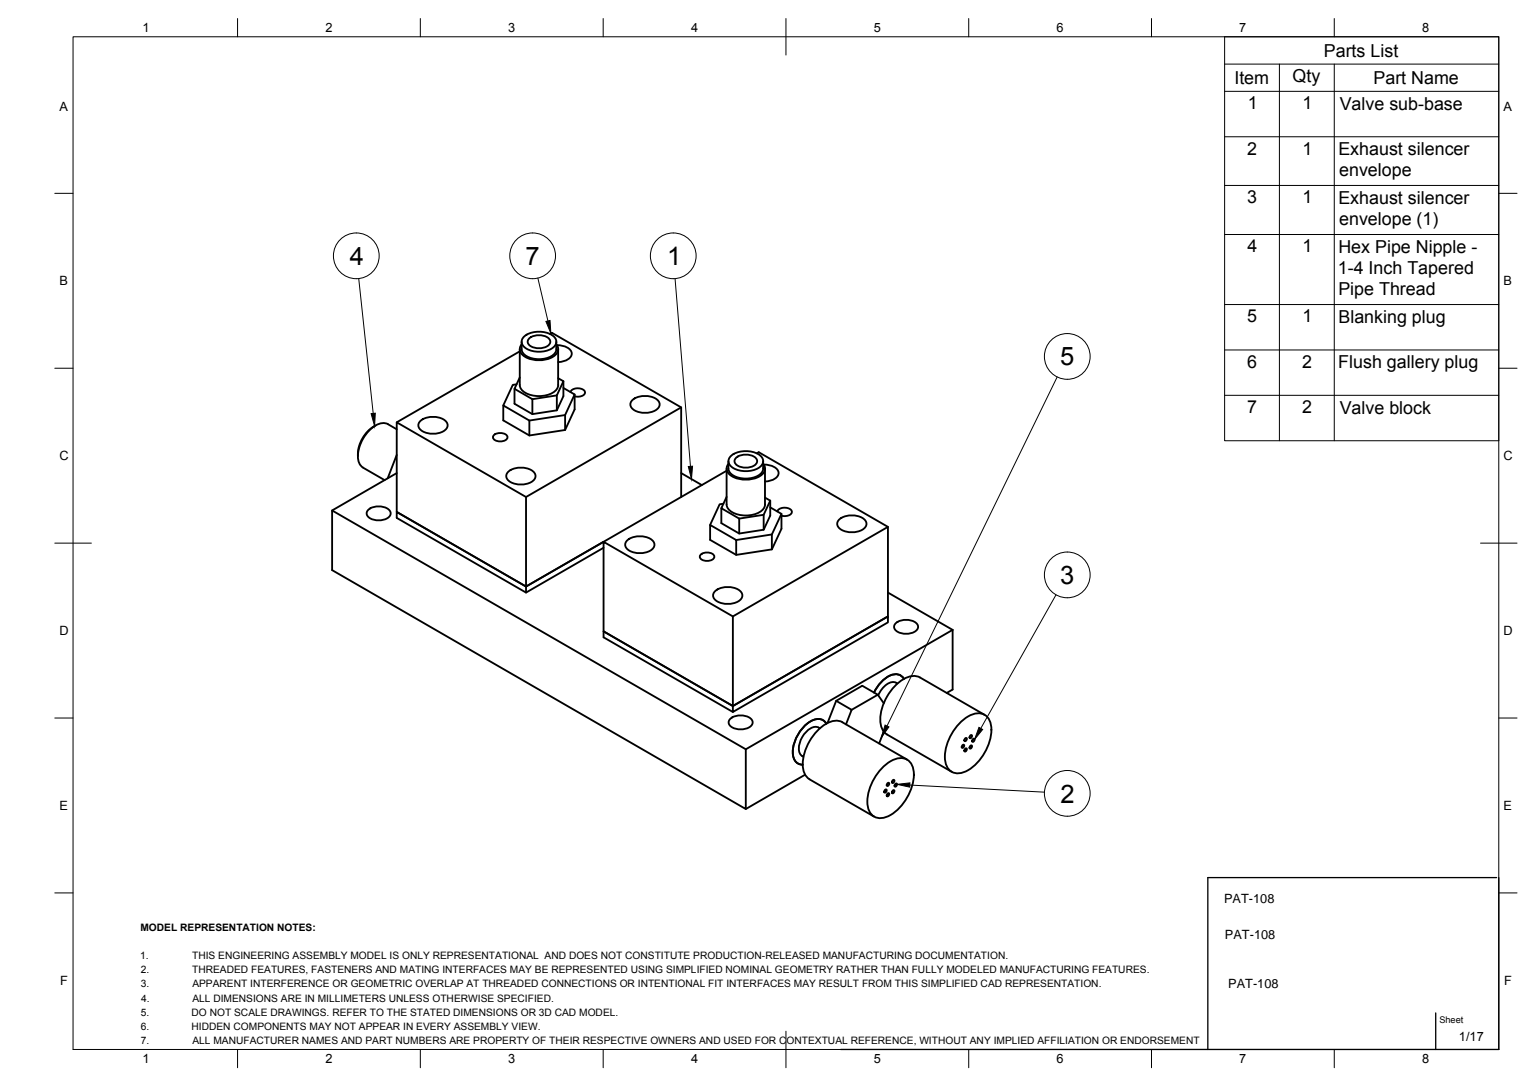
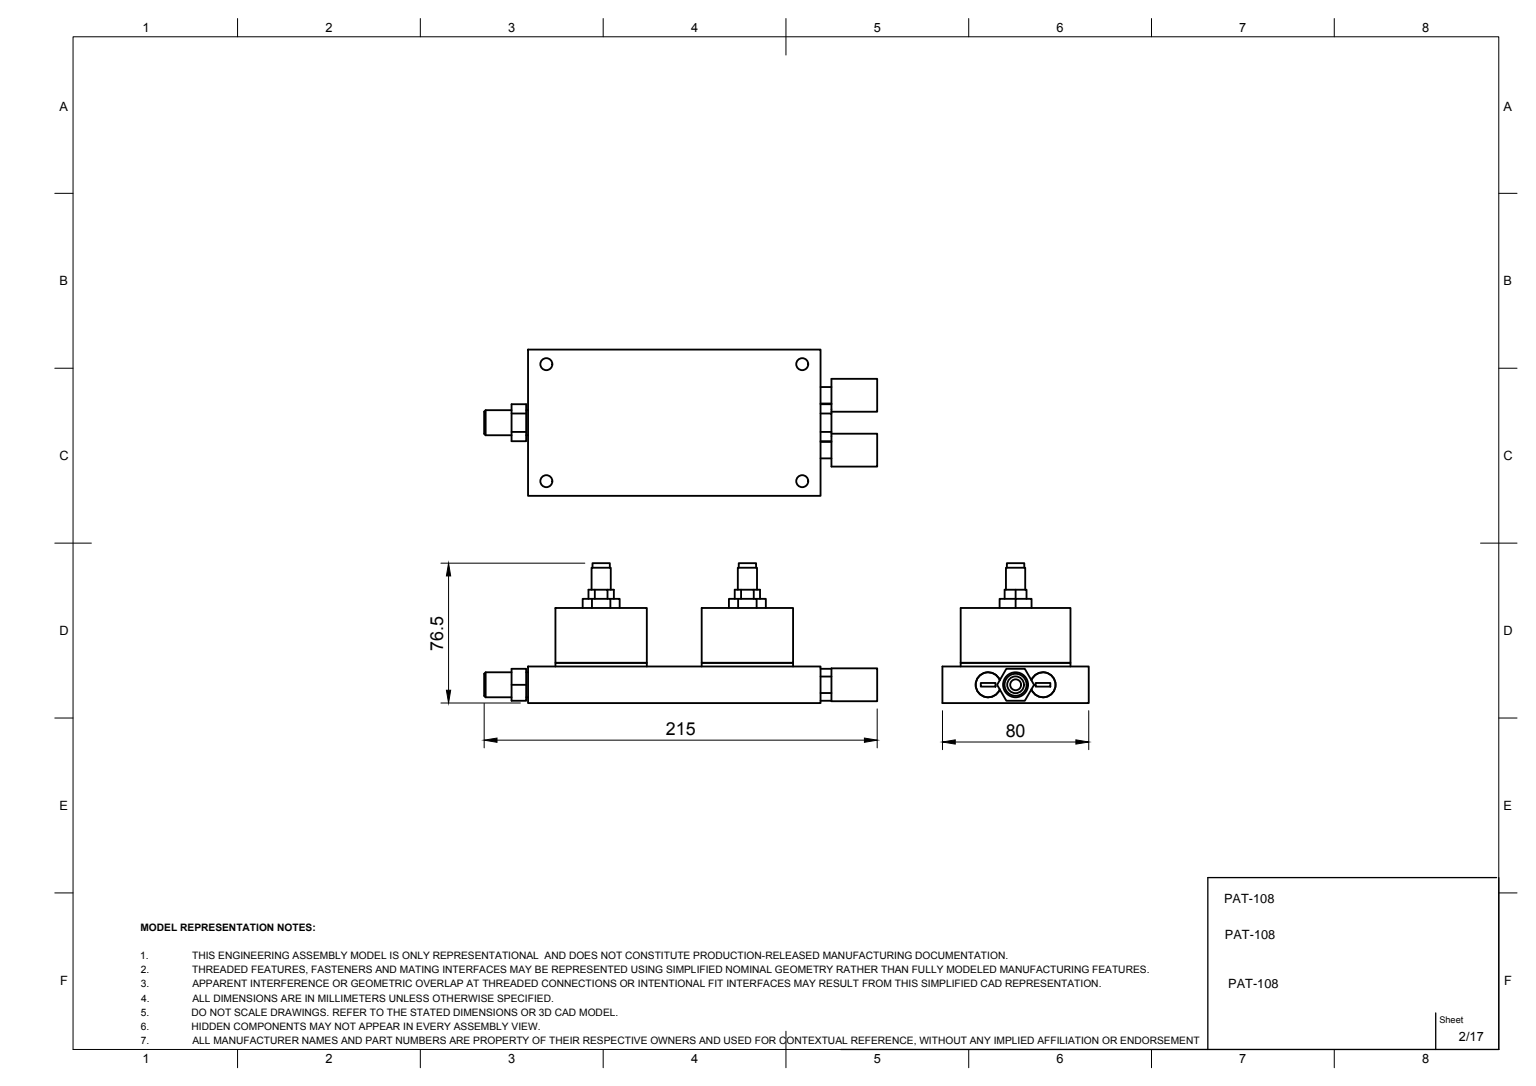
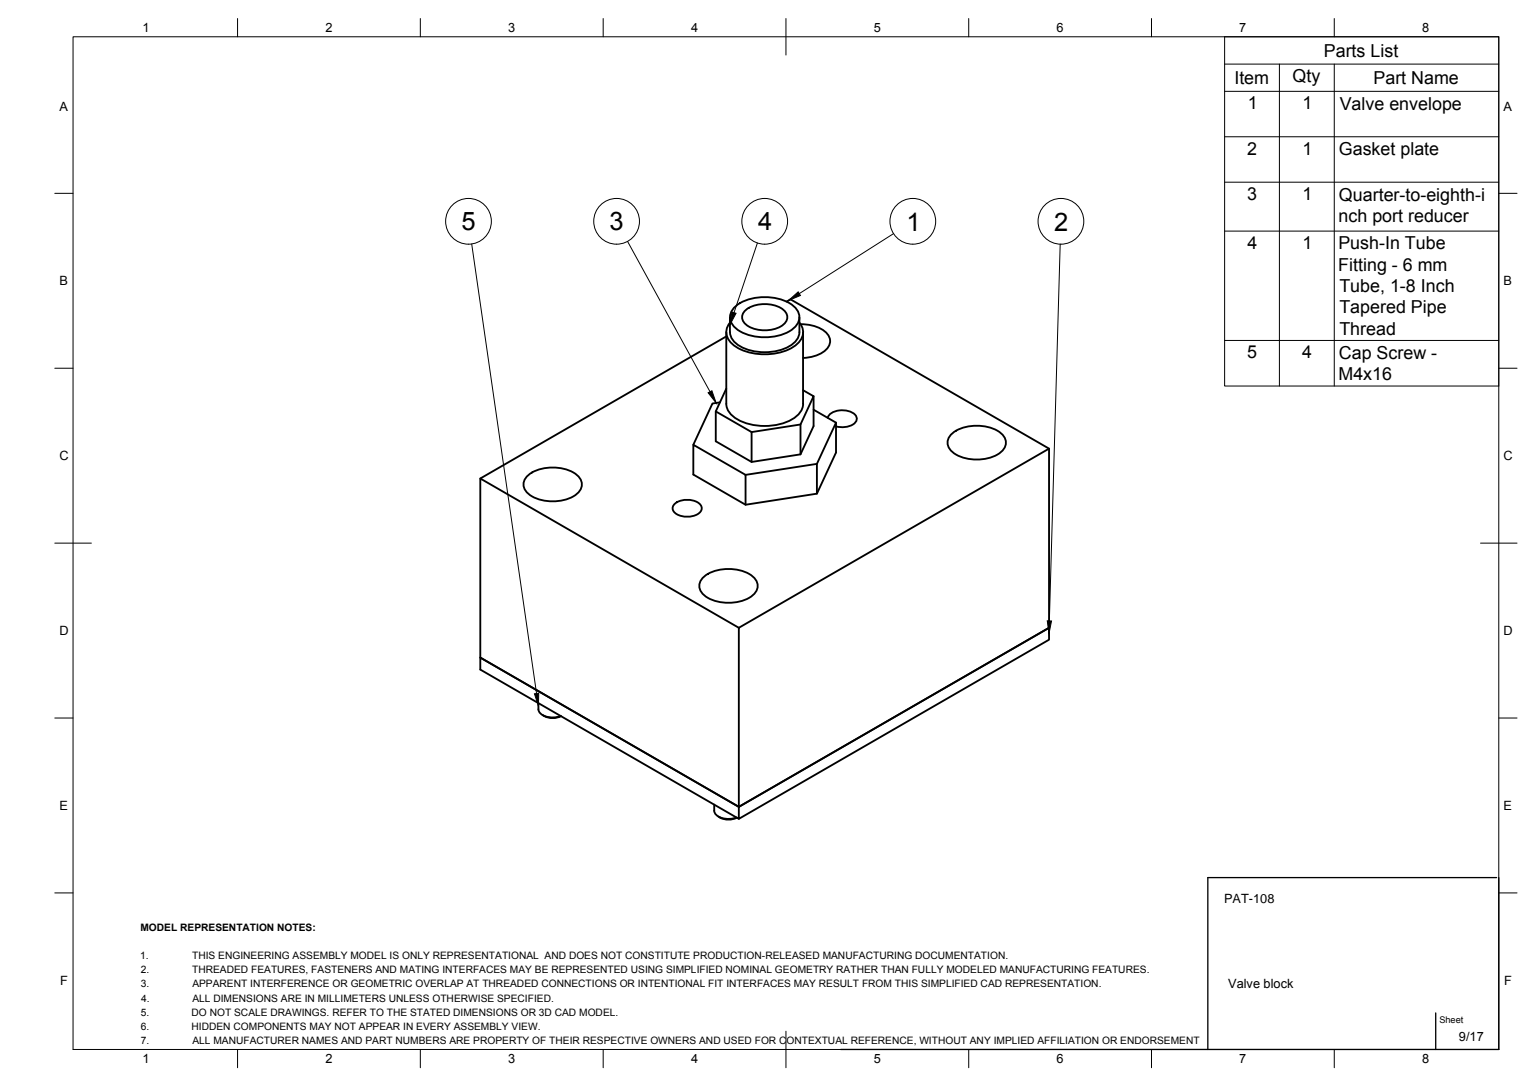
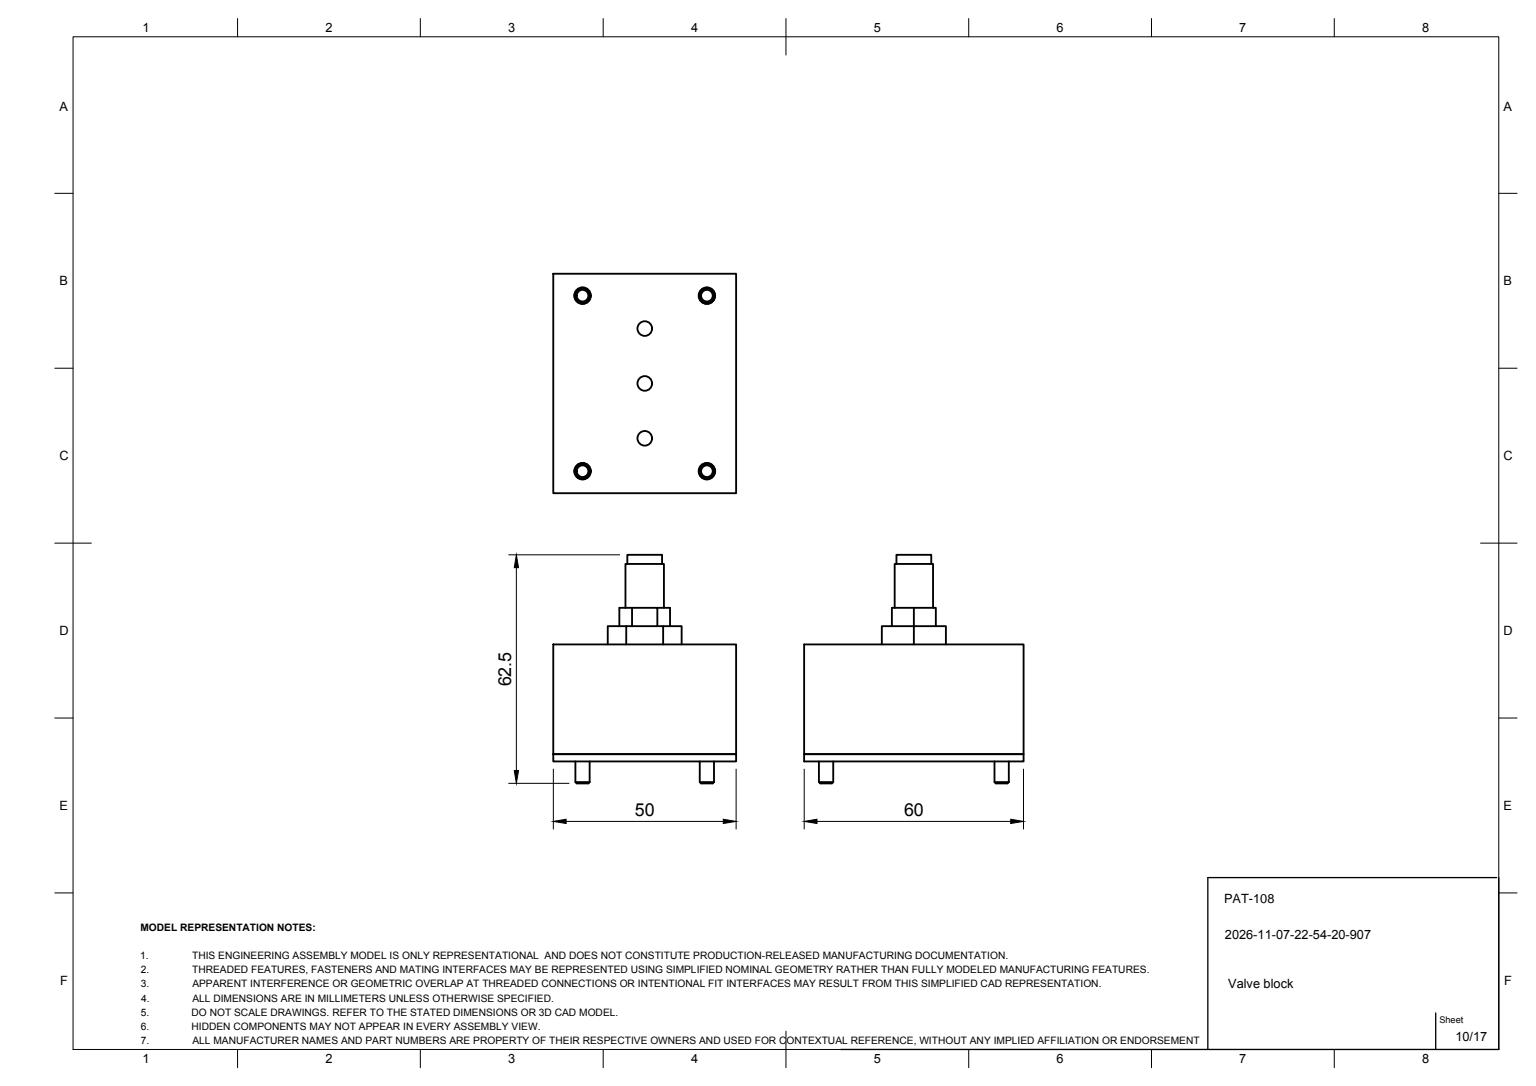
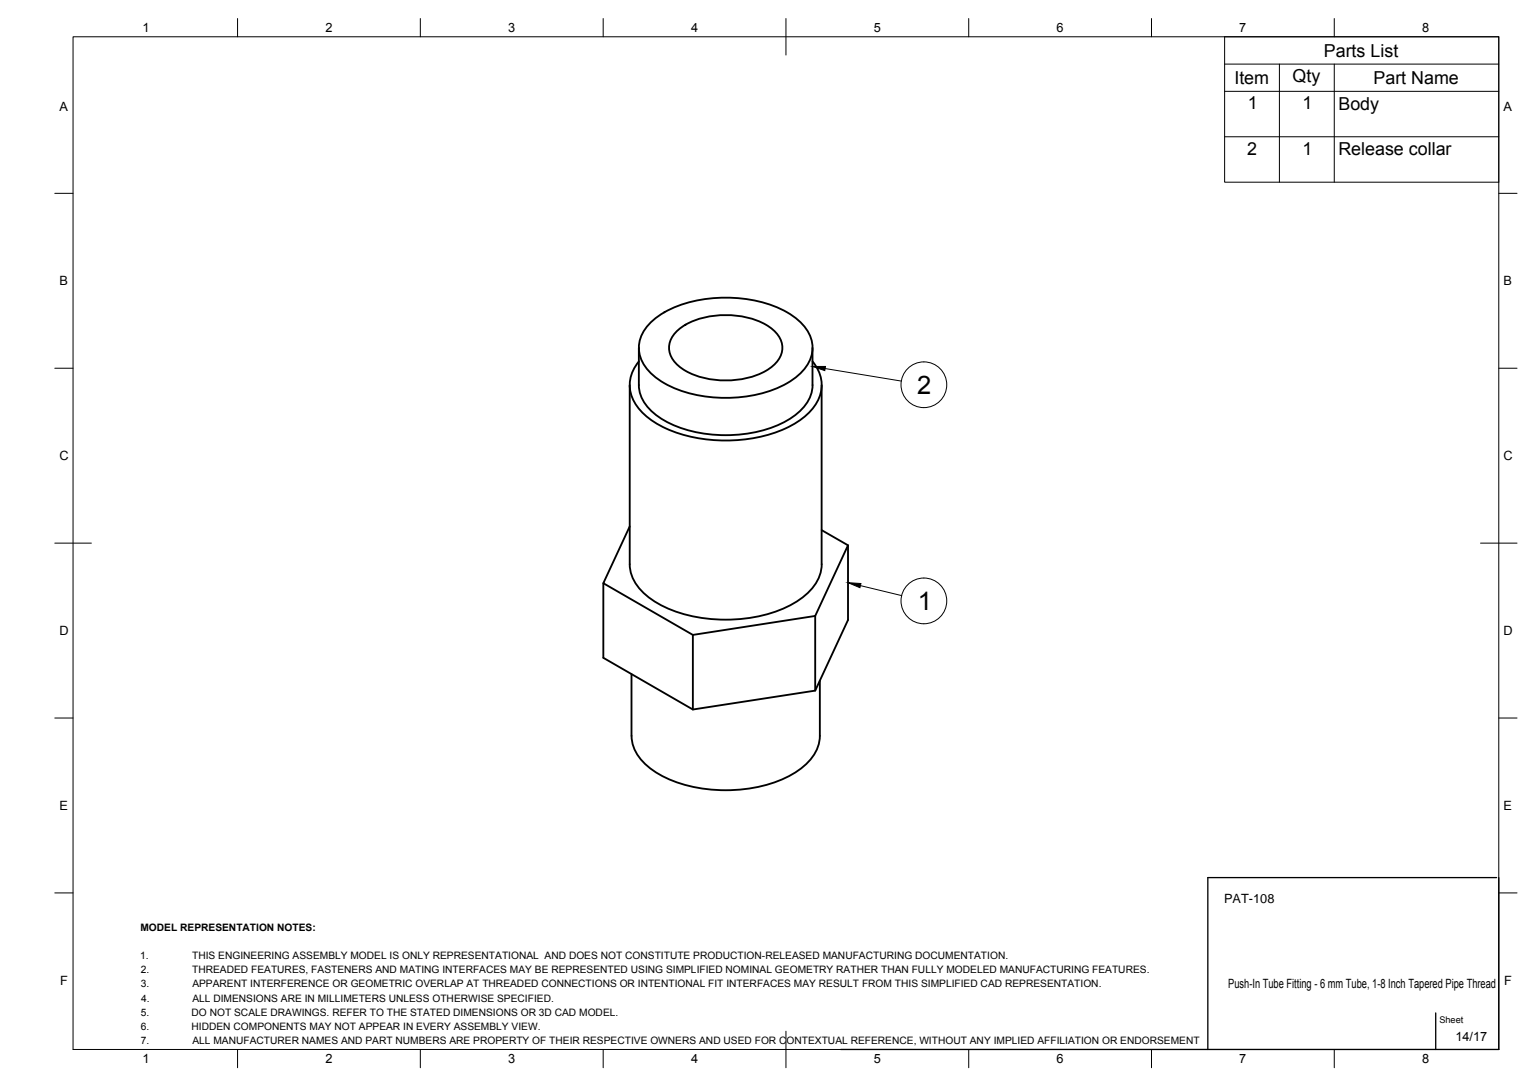
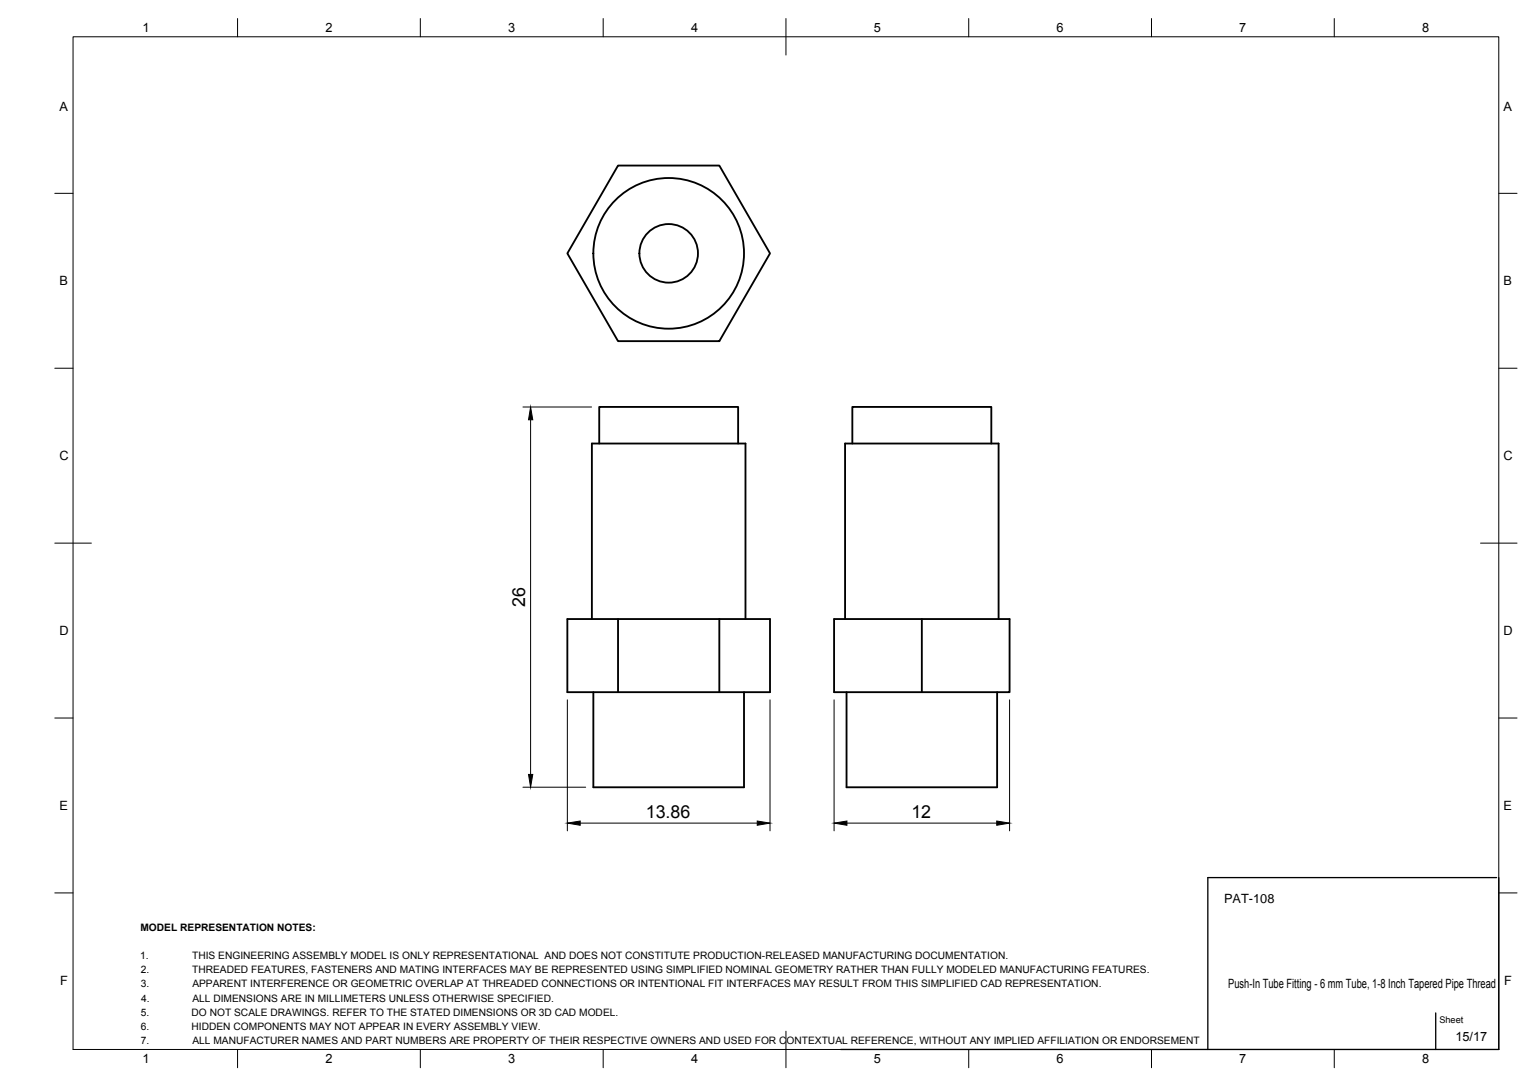
ISO-10303-21;
HEADER;
/* Generated by software containing ST-Developer
 * from STEP Tools, Inc. (www.steptools.com) 
 */

FILE_DESCRIPTION(
/* description */ ('Sub-base valve envelopes and connections'),
/* implementation_level */ '2;1');

FILE_NAME(
/* name */ 'PAT-108',
/* time_stamp */ '2026-10-29T15:55:44-07:00',
/* author */ (''),
/* organization */ (''),
/* preprocessor_version */ 'ST-DEVELOPER v20.2',
/* originating_system */ 'Autodesk Translation Framework v15.17.0.0',
/* authorisation */ '');

FILE_SCHEMA (('AUTOMOTIVE_DESIGN { 1 0 10303 214 3 1 1 }'));
ENDSEC;

DATA;
#10=MECHANICAL_DESIGN_GEOMETRIC_PRESENTATION_REPRESENTATION('',(#119,#120,
#121,#122,#123,#124,#125,#126,#127,#128,#129,#130),#6113);
#11=ORIENTED_CLOSED_SHELL('',*,#3370,.F.);
#12=BREP_WITH_VOIDS('Body1',#3369,(#11));
#13=ITEM_DEFINED_TRANSFORMATION($,$,#3819,#3860);
#14=ITEM_DEFINED_TRANSFORMATION($,$,#3847,#3861);
#15=ITEM_DEFINED_TRANSFORMATION($,$,#3722,#3888);
#16=ITEM_DEFINED_TRANSFORMATION($,$,#3770,#3889);
#17=ITEM_DEFINED_TRANSFORMATION($,$,#3798,#3890);
#18=ITEM_DEFINED_TRANSFORMATION($,$,#3818,#3891);
#19=ITEM_DEFINED_TRANSFORMATION($,$,#3862,#3892);
#20=ITEM_DEFINED_TRANSFORMATION($,$,#3862,#3893);
#21=ITEM_DEFINED_TRANSFORMATION($,$,#3862,#3894);
#22=ITEM_DEFINED_TRANSFORMATION($,$,#3862,#3895);
#23=ITEM_DEFINED_TRANSFORMATION($,$,#3505,#3896);
#24=ITEM_DEFINED_TRANSFORMATION($,$,#3601,#3897);
#25=ITEM_DEFINED_TRANSFORMATION($,$,#3637,#3898);
#26=ITEM_DEFINED_TRANSFORMATION($,$,#3673,#3899);
#27=ITEM_DEFINED_TRANSFORMATION($,$,#3697,#3900);
#28=ITEM_DEFINED_TRANSFORMATION($,$,#3710,#3901);
#29=ITEM_DEFINED_TRANSFORMATION($,$,#3710,#3902);
#30=ITEM_DEFINED_TRANSFORMATION($,$,#3721,#3903);
#31=ITEM_DEFINED_TRANSFORMATION($,$,#3721,#3904);
#32=(
REPRESENTATION_RELATIONSHIP($,$,#6179,#6178)
REPRESENTATION_RELATIONSHIP_WITH_TRANSFORMATION(#13)
SHAPE_REPRESENTATION_RELATIONSHIP()
);
#33=(
REPRESENTATION_RELATIONSHIP($,$,#6180,#6178)
REPRESENTATION_RELATIONSHIP_WITH_TRANSFORMATION(#14)
SHAPE_REPRESENTATION_RELATIONSHIP()
);
#34=(
REPRESENTATION_RELATIONSHIP($,$,#6175,#6174)
REPRESENTATION_RELATIONSHIP_WITH_TRANSFORMATION(#15)
SHAPE_REPRESENTATION_RELATIONSHIP()
);
#35=(
REPRESENTATION_RELATIONSHIP($,$,#6176,#6174)
REPRESENTATION_RELATIONSHIP_WITH_TRANSFORMATION(#16)
SHAPE_REPRESENTATION_RELATIONSHIP()
);
#36=(
REPRESENTATION_RELATIONSHIP($,$,#6177,#6174)
REPRESENTATION_RELATIONSHIP_WITH_TRANSFORMATION(#17)
SHAPE_REPRESENTATION_RELATIONSHIP()
);
#37=(
REPRESENTATION_RELATIONSHIP($,$,#6178,#6174)
REPRESENTATION_RELATIONSHIP_WITH_TRANSFORMATION(#18)
SHAPE_REPRESENTATION_RELATIONSHIP()
);
#38=(
REPRESENTATION_RELATIONSHIP($,$,#6181,#6174)
REPRESENTATION_RELATIONSHIP_WITH_TRANSFORMATION(#19)
SHAPE_REPRESENTATION_RELATIONSHIP()
);
#39=(
REPRESENTATION_RELATIONSHIP($,$,#6181,#6174)
REPRESENTATION_RELATIONSHIP_WITH_TRANSFORMATION(#20)
SHAPE_REPRESENTATION_RELATIONSHIP()
);
#40=(
REPRESENTATION_RELATIONSHIP($,$,#6181,#6174)
REPRESENTATION_RELATIONSHIP_WITH_TRANSFORMATION(#21)
SHAPE_REPRESENTATION_RELATIONSHIP()
);
#41=(
REPRESENTATION_RELATIONSHIP($,$,#6181,#6174)
REPRESENTATION_RELATIONSHIP_WITH_TRANSFORMATION(#22)
SHAPE_REPRESENTATION_RELATIONSHIP()
);
#42=(
REPRESENTATION_RELATIONSHIP($,$,#6168,#6167)
REPRESENTATION_RELATIONSHIP_WITH_TRANSFORMATION(#23)
SHAPE_REPRESENTATION_RELATIONSHIP()
);
#43=(
REPRESENTATION_RELATIONSHIP($,$,#6169,#6167)
REPRESENTATION_RELATIONSHIP_WITH_TRANSFORMATION(#24)
SHAPE_REPRESENTATION_RELATIONSHIP()
);
#44=(
REPRESENTATION_RELATIONSHIP($,$,#6170,#6167)
REPRESENTATION_RELATIONSHIP_WITH_TRANSFORMATION(#25)
SHAPE_REPRESENTATION_RELATIONSHIP()
);
#45=(
REPRESENTATION_RELATIONSHIP($,$,#6171,#6167)
REPRESENTATION_RELATIONSHIP_WITH_TRANSFORMATION(#26)
SHAPE_REPRESENTATION_RELATIONSHIP()
);
#46=(
REPRESENTATION_RELATIONSHIP($,$,#6172,#6167)
REPRESENTATION_RELATIONSHIP_WITH_TRANSFORMATION(#27)
SHAPE_REPRESENTATION_RELATIONSHIP()
);
#47=(
REPRESENTATION_RELATIONSHIP($,$,#6173,#6167)
REPRESENTATION_RELATIONSHIP_WITH_TRANSFORMATION(#28)
SHAPE_REPRESENTATION_RELATIONSHIP()
);
#48=(
REPRESENTATION_RELATIONSHIP($,$,#6173,#6167)
REPRESENTATION_RELATIONSHIP_WITH_TRANSFORMATION(#29)
SHAPE_REPRESENTATION_RELATIONSHIP()
);
#49=(
REPRESENTATION_RELATIONSHIP($,$,#6174,#6167)
REPRESENTATION_RELATIONSHIP_WITH_TRANSFORMATION(#30)
SHAPE_REPRESENTATION_RELATIONSHIP()
);
#50=(
REPRESENTATION_RELATIONSHIP($,$,#6174,#6167)
REPRESENTATION_RELATIONSHIP_WITH_TRANSFORMATION(#31)
SHAPE_REPRESENTATION_RELATIONSHIP()
);
#51=CONTEXT_DEPENDENT_SHAPE_REPRESENTATION(#32,#6147);
#52=CONTEXT_DEPENDENT_SHAPE_REPRESENTATION(#33,#6148);
#53=CONTEXT_DEPENDENT_SHAPE_REPRESENTATION(#34,#6150);
#54=CONTEXT_DEPENDENT_SHAPE_REPRESENTATION(#35,#6151);
#55=CONTEXT_DEPENDENT_SHAPE_REPRESENTATION(#36,#6152);
#56=CONTEXT_DEPENDENT_SHAPE_REPRESENTATION(#37,#6153);
#57=CONTEXT_DEPENDENT_SHAPE_REPRESENTATION(#38,#6154);
#58=CONTEXT_DEPENDENT_SHAPE_REPRESENTATION(#39,#6155);
#59=CONTEXT_DEPENDENT_SHAPE_REPRESENTATION(#40,#6156);
#60=CONTEXT_DEPENDENT_SHAPE_REPRESENTATION(#41,#6157);
#61=CONTEXT_DEPENDENT_SHAPE_REPRESENTATION(#42,#6158);
#62=CONTEXT_DEPENDENT_SHAPE_REPRESENTATION(#43,#6159);
#63=CONTEXT_DEPENDENT_SHAPE_REPRESENTATION(#44,#6160);
#64=CONTEXT_DEPENDENT_SHAPE_REPRESENTATION(#45,#6161);
#65=CONTEXT_DEPENDENT_SHAPE_REPRESENTATION(#46,#6162);
#66=CONTEXT_DEPENDENT_SHAPE_REPRESENTATION(#47,#6163);
#67=CONTEXT_DEPENDENT_SHAPE_REPRESENTATION(#48,#6164);
#68=CONTEXT_DEPENDENT_SHAPE_REPRESENTATION(#49,#6165);
#69=CONTEXT_DEPENDENT_SHAPE_REPRESENTATION(#50,#6166);
#70=NEXT_ASSEMBLY_USAGE_OCCURRENCE('Body:1','Body:1','Body:1',#6194,#6195,
'Body:1');
#71=NEXT_ASSEMBLY_USAGE_OCCURRENCE('Release collar:1',
'Release collar:1','Release collar:1',#6194,#6196,'Release collar:1');
#72=NEXT_ASSEMBLY_USAGE_OCCURRENCE('Valve envelope:1',
'Valve envelope:1','Valve envelope:1',#6190,#6191,'Valve envelope:1');
#73=NEXT_ASSEMBLY_USAGE_OCCURRENCE('Gasket plate:1','Gasket plate:1',
'Gasket plate:1',#6190,#6192,'Gasket plate:1');
#74=NEXT_ASSEMBLY_USAGE_OCCURRENCE(
'Quarter-to-eighth-inch port reducer:1',
'Quarter-to-eighth-inch port reducer:1',
'Quarter-to-eighth-inch port reducer:1',#6190,#6193,
'Quarter-to-eighth-inch port reducer:1');
#75=NEXT_ASSEMBLY_USAGE_OCCURRENCE(
'Push-In Tube Fitting - 6 mm Tube, 1-8 Inch Tapered Pipe Thread:1',
'Push-In Tube Fitting - 6 mm Tube, 1-8 Inch Tapered Pipe Thread:1',
'Push-In Tube Fitting - 6 mm Tube, 1-8 Inch Tapered Pipe Thread:1',#6190,
#6194,
'Push-In Tube Fitting - 6 mm Tube, 1-8 Inch Tapered Pipe Thread:1');
#76=NEXT_ASSEMBLY_USAGE_OCCURRENCE('Cap Screw - M4x16:1',
'Cap Screw - M4x16:1','Cap Screw - M4x16:1',#6190,#6197,
'Cap Screw - M4x16:1');
#77=NEXT_ASSEMBLY_USAGE_OCCURRENCE('Cap Screw - M4x16:4',
'Cap Screw - M4x16:4','Cap Screw - M4x16:4',#6190,#6197,
'Cap Screw - M4x16:4');
#78=NEXT_ASSEMBLY_USAGE_OCCURRENCE('Cap Screw - M4x16:3',
'Cap Screw - M4x16:3','Cap Screw - M4x16:3',#6190,#6197,
'Cap Screw - M4x16:3');
#79=NEXT_ASSEMBLY_USAGE_OCCURRENCE('Cap Screw - M4x16:2',
'Cap Screw - M4x16:2','Cap Screw - M4x16:2',#6190,#6197,
'Cap Screw - M4x16:2');
#80=NEXT_ASSEMBLY_USAGE_OCCURRENCE('Valve sub-base:1',
'Valve sub-base:1','Valve sub-base:1',#6183,#6184,'Valve sub-base:1');
#81=NEXT_ASSEMBLY_USAGE_OCCURRENCE('Exhaust silencer envelope:1',
'Exhaust silencer envelope:1','Exhaust silencer envelope:1',#6183,#6185,
'Exhaust silencer envelope:1');
#82=NEXT_ASSEMBLY_USAGE_OCCURRENCE('Exhaust silencer envelope (1):1',
'Exhaust silencer envelope (1):1','Exhaust silencer envelope (1):1',#6183,
#6186,'Exhaust silencer envelope (1):1');
#83=NEXT_ASSEMBLY_USAGE_OCCURRENCE(
'Hex Pipe Nipple - 1-4 Inch Tapered Pipe Thread:1',
'Hex Pipe Nipple - 1-4 Inch Tapered Pipe Thread:1',
'Hex Pipe Nipple - 1-4 Inch Tapered Pipe Thread:1',#6183,#6187,
'Hex Pipe Nipple - 1-4 Inch Tapered Pipe Thread:1');
#84=NEXT_ASSEMBLY_USAGE_OCCURRENCE('Blanking plug:1','Blanking plug:1',
'Blanking plug:1',#6183,#6188,'Blanking plug:1');
#85=NEXT_ASSEMBLY_USAGE_OCCURRENCE('Flush gallery plug:1',
'Flush gallery plug:1','Flush gallery plug:1',#6183,#6189,
'Flush gallery plug:1');
#86=NEXT_ASSEMBLY_USAGE_OCCURRENCE('Flush gallery plug:2',
'Flush gallery plug:2','Flush gallery plug:2',#6183,#6189,
'Flush gallery plug:2');
#87=NEXT_ASSEMBLY_USAGE_OCCURRENCE('Valve block:1','Valve block:1',
'Valve block:1',#6183,#6190,'Valve block:1');
#88=NEXT_ASSEMBLY_USAGE_OCCURRENCE('Valve block:2','Valve block:2',
'Valve block:2',#6183,#6190,'Valve block:2');
#89=CONICAL_SURFACE('',#3689,0.645,0.785398163397448);
#90=CONICAL_SURFACE('',#3692,0.645,0.785398163397448);
#91=CONICAL_SURFACE('',#3865,0.325,0.785398163397448);
#92=CONICAL_SURFACE('',#3869,0.335,0.785398163397448);
#93=CONICAL_SURFACE('',#3873,0.21,0.463647609000806);
#94=CONICAL_SURFACE('',#3877,0.18,0.785398163397448);
#95=SHAPE_REPRESENTATION_RELATIONSHIP('SRR','None',#6168,#107);
#96=SHAPE_REPRESENTATION_RELATIONSHIP('SRR','None',#6169,#108);
#97=SHAPE_REPRESENTATION_RELATIONSHIP('SRR','None',#6170,#109);
#98=SHAPE_REPRESENTATION_RELATIONSHIP('SRR','None',#6171,#110);
#99=SHAPE_REPRESENTATION_RELATIONSHIP('SRR','None',#6172,#111);
#100=SHAPE_REPRESENTATION_RELATIONSHIP('SRR','None',#6173,#112);
#101=SHAPE_REPRESENTATION_RELATIONSHIP('SRR','None',#6175,#113);
#102=SHAPE_REPRESENTATION_RELATIONSHIP('SRR','None',#6176,#114);
#103=SHAPE_REPRESENTATION_RELATIONSHIP('SRR','None',#6177,#115);
#104=SHAPE_REPRESENTATION_RELATIONSHIP('SRR','None',#6179,#116);
#105=SHAPE_REPRESENTATION_RELATIONSHIP('SRR','None',#6180,#117);
#106=SHAPE_REPRESENTATION_RELATIONSHIP('SRR','None',#6181,#118);
#107=ADVANCED_BREP_SHAPE_REPRESENTATION('',(#131),#6099);
#108=ADVANCED_BREP_SHAPE_REPRESENTATION('',(#132),#6100);
#109=ADVANCED_BREP_SHAPE_REPRESENTATION('',(#133),#6101);
#110=ADVANCED_BREP_SHAPE_REPRESENTATION('',(#134),#6102);
#111=ADVANCED_BREP_SHAPE_REPRESENTATION('',(#135),#6103);
#112=ADVANCED_BREP_SHAPE_REPRESENTATION('',(#136),#6104);
#113=ADVANCED_BREP_SHAPE_REPRESENTATION('',(#137),#6106);
#114=ADVANCED_BREP_SHAPE_REPRESENTATION('',(#138),#6107);
#115=ADVANCED_BREP_SHAPE_REPRESENTATION('',(#139),#6108);
#116=ADVANCED_BREP_SHAPE_REPRESENTATION('',(#140),#6110);
#117=ADVANCED_BREP_SHAPE_REPRESENTATION('',(#141),#6111);
#118=ADVANCED_BREP_SHAPE_REPRESENTATION('',(#12),#6112);
#119=STYLED_ITEM('',(#6294),#131);
#120=STYLED_ITEM('',(#6329),#132);
#121=STYLED_ITEM('',(#6329),#133);
#122=STYLED_ITEM('',(#6308),#134);
#123=STYLED_ITEM('',(#6329),#135);
#124=STYLED_ITEM('',(#6329),#136);
#125=STYLED_ITEM('',(#6301),#137);
#126=STYLED_ITEM('',(#6329),#138);
#127=STYLED_ITEM('',(#6301),#139);
#128=STYLED_ITEM('',(#6294),#140);
#129=STYLED_ITEM('',(#6329),#141);
#130=STYLED_ITEM('',(#6322),#12);
#131=MANIFOLD_SOLID_BREP('Body1',#3358);
#132=MANIFOLD_SOLID_BREP('Body1',#3359);
#133=MANIFOLD_SOLID_BREP('Body1',#3360);
#134=MANIFOLD_SOLID_BREP('Body1',#3361);
#135=MANIFOLD_SOLID_BREP('Body1',#3362);
#136=MANIFOLD_SOLID_BREP('Body1',#3363);
#137=MANIFOLD_SOLID_BREP('Body1',#3364);
#138=MANIFOLD_SOLID_BREP('Body1',#3365);
#139=MANIFOLD_SOLID_BREP('Body1',#3366);
#140=MANIFOLD_SOLID_BREP('Body1',#3367);
#141=MANIFOLD_SOLID_BREP('Body1',#3368);
#142=FACE_BOUND('',#613,.T.);
#143=FACE_BOUND('',#616,.T.);
#144=FACE_BOUND('',#619,.T.);
#145=FACE_BOUND('',#622,.T.);
#146=FACE_BOUND('',#625,.T.);
#147=FACE_BOUND('',#628,.T.);
#148=FACE_BOUND('',#634,.T.);
#149=FACE_BOUND('',#635,.T.);
#150=FACE_BOUND('',#636,.T.);
#151=FACE_BOUND('',#639,.T.);
#152=FACE_BOUND('',#640,.T.);
#153=FACE_BOUND('',#641,.T.);
#154=FACE_BOUND('',#643,.T.);
#155=FACE_BOUND('',#644,.T.);
#156=FACE_BOUND('',#645,.T.);
#157=FACE_BOUND('',#646,.T.);
#158=FACE_BOUND('',#647,.T.);
#159=FACE_BOUND('',#648,.T.);
#160=FACE_BOUND('',#649,.T.);
#161=FACE_BOUND('',#650,.T.);
#162=FACE_BOUND('',#651,.T.);
#163=FACE_BOUND('',#652,.T.);
#164=FACE_BOUND('',#653,.T.);
#165=FACE_BOUND('',#654,.T.);
#166=FACE_BOUND('',#655,.T.);
#167=FACE_BOUND('',#656,.T.);
#168=FACE_BOUND('',#657,.T.);
#169=FACE_BOUND('',#658,.T.);
#170=FACE_BOUND('',#659,.T.);
#171=FACE_BOUND('',#660,.T.);
#172=FACE_BOUND('',#662,.T.);
#173=FACE_BOUND('',#663,.T.);
#174=FACE_BOUND('',#664,.T.);
#175=FACE_BOUND('',#665,.T.);
#176=FACE_BOUND('',#673,.T.);
#177=FACE_BOUND('',#674,.T.);
#178=FACE_BOUND('',#675,.T.);
#179=FACE_BOUND('',#676,.T.);
#180=FACE_BOUND('',#677,.T.);
#181=FACE_BOUND('',#678,.T.);
#182=FACE_BOUND('',#680,.T.);
#183=FACE_BOUND('',#683,.T.);
#184=FACE_BOUND('',#684,.T.);
#185=FACE_BOUND('',#685,.T.);
#186=FACE_BOUND('',#686,.T.);
#187=FACE_BOUND('',#687,.T.);
#188=FACE_BOUND('',#688,.T.);
#189=FACE_BOUND('',#693,.T.);
#190=FACE_BOUND('',#695,.T.);
#191=FACE_BOUND('',#703,.T.);
#192=FACE_BOUND('',#704,.T.);
#193=FACE_BOUND('',#705,.T.);
#194=FACE_BOUND('',#706,.T.);
#195=FACE_BOUND('',#707,.T.);
#196=FACE_BOUND('',#708,.T.);
#197=FACE_BOUND('',#710,.T.);
#198=FACE_BOUND('',#713,.T.);
#199=FACE_BOUND('',#714,.T.);
#200=FACE_BOUND('',#715,.T.);
#201=FACE_BOUND('',#716,.T.);
#202=FACE_BOUND('',#717,.T.);
#203=FACE_BOUND('',#718,.T.);
#204=FACE_BOUND('',#723,.T.);
#205=FACE_BOUND('',#725,.T.);
#206=FACE_BOUND('',#727,.T.);
#207=FACE_BOUND('',#729,.T.);
#208=FACE_BOUND('',#738,.T.);
#209=FACE_BOUND('',#743,.T.);
#210=FACE_BOUND('',#746,.T.);
#211=FACE_BOUND('',#762,.T.);
#212=FACE_BOUND('',#767,.T.);
#213=FACE_BOUND('',#770,.T.);
#214=FACE_BOUND('',#773,.T.);
#215=FACE_BOUND('',#776,.T.);
#216=FACE_BOUND('',#783,.T.);
#217=FACE_BOUND('',#792,.T.);
#218=FACE_BOUND('',#793,.T.);
#219=FACE_BOUND('',#794,.T.);
#220=FACE_BOUND('',#795,.T.);
#221=FACE_BOUND('',#796,.T.);
#222=FACE_BOUND('',#797,.T.);
#223=FACE_BOUND('',#798,.T.);
#224=FACE_BOUND('',#800,.T.);
#225=FACE_BOUND('',#801,.T.);
#226=FACE_BOUND('',#802,.T.);
#227=FACE_BOUND('',#803,.T.);
#228=FACE_BOUND('',#804,.T.);
#229=FACE_BOUND('',#805,.T.);
#230=FACE_BOUND('',#806,.T.);
#231=FACE_BOUND('',#819,.T.);
#232=FACE_BOUND('',#820,.T.);
#233=FACE_BOUND('',#821,.T.);
#234=FACE_BOUND('',#822,.T.);
#235=FACE_BOUND('',#823,.T.);
#236=FACE_BOUND('',#824,.T.);
#237=FACE_BOUND('',#825,.T.);
#238=FACE_BOUND('',#827,.T.);
#239=FACE_BOUND('',#828,.T.);
#240=FACE_BOUND('',#829,.T.);
#241=FACE_BOUND('',#830,.T.);
#242=FACE_BOUND('',#831,.T.);
#243=FACE_BOUND('',#832,.T.);
#244=FACE_BOUND('',#833,.T.);
#245=FACE_BOUND('',#836,.T.);
#246=FACE_BOUND('',#838,.T.);
#247=FACE_BOUND('',#846,.T.);
#248=FACE_BOUND('',#850,.T.);
#249=FACE_BOUND('',#853,.T.);
#250=FACE_BOUND('',#855,.T.);
#251=FACE_BOUND('',#857,.T.);
#252=FACE_BOUND('',#865,.T.);
#253=FACE_BOUND('',#868,.T.);
#254=FACE_BOUND('',#872,.T.);
#255=FACE_BOUND('',#875,.T.);
#256=FACE_BOUND('',#878,.T.);
#257=FACE_BOUND('',#881,.T.);
#258=FACE_BOUND('',#888,.T.);
#259=B_SPLINE_CURVE_WITH_KNOTS('',3,(#4974,#4975,#4976,#4977,#4978,#4979,
#4980,#4981,#4982,#4983),.UNSPECIFIED.,.F.,.F.,(4,2,2,2,4),(0.,0.0789054703932594,
0.157810940786519,0.235848341776527,0.313885742766534),.UNSPECIFIED.);
#260=B_SPLINE_CURVE_WITH_KNOTS('',3,(#4985,#4986,#4987,#4988,#4989,#4990,
#4991,#4992,#4993,#4994),.UNSPECIFIED.,.F.,.F.,(4,2,2,2,4),(0.941657228299604,
1.01969462928961,1.09773203027962,1.17663750067288,1.25554297106614),
 .UNSPECIFIED.);
#261=B_SPLINE_CURVE_WITH_KNOTS('',3,(#4998,#4999,#5000,#5001,#5002,#5003,
#5004,#5005,#5006,#5007,#5008,#5009,#5010,#5011,#5012,#5013,#5014,#5015),
 .UNSPECIFIED.,.F.,.F.,(4,2,2,2,2,2,2,2,4),(0.313885742766534,0.391923143756543,
0.469960544746551,0.54886601513981,0.627771485533069,0.706676955926329,
0.785582426319588,0.863619827309596,0.941657228299604),.UNSPECIFIED.);
#262=B_SPLINE_CURVE_WITH_KNOTS('',3,(#5019,#5020,#5021,#5022,#5023,#5024,
#5025,#5026,#5027,#5028),.UNSPECIFIED.,.F.,.F.,(4,2,2,2,4),(0.,0.0789054703932594,
0.157810940786519,0.235848341776527,0.313885742766535),.UNSPECIFIED.);
#263=B_SPLINE_CURVE_WITH_KNOTS('',3,(#5030,#5031,#5032,#5033,#5034,#5035,
#5036,#5037,#5038,#5039),.UNSPECIFIED.,.F.,.F.,(4,2,2,2,4),(0.941657228299605,
1.01969462928961,1.09773203027962,1.17663750067288,1.25554297106614),
 .UNSPECIFIED.);
#264=B_SPLINE_CURVE_WITH_KNOTS('',3,(#5043,#5044,#5045,#5046,#5047,#5048,
#5049,#5050,#5051,#5052,#5053,#5054,#5055,#5056,#5057,#5058,#5059,#5060),
 .UNSPECIFIED.,.F.,.F.,(4,2,2,2,2,2,2,2,4),(0.313885742766535,0.391923143756543,
0.469960544746551,0.54886601513981,0.627771485533069,0.706676955926329,
0.785582426319588,0.863619827309597,0.941657228299605),.UNSPECIFIED.);
#265=B_SPLINE_CURVE_WITH_KNOTS('',3,(#5064,#5065,#5066,#5067,#5068,#5069,
#5070,#5071,#5072,#5073),.UNSPECIFIED.,.F.,.F.,(4,2,2,2,4),(0.,0.0789054703932594,
0.157810940786519,0.235848341776527,0.313885742766534),.UNSPECIFIED.);
#266=B_SPLINE_CURVE_WITH_KNOTS('',3,(#5075,#5076,#5077,#5078,#5079,#5080,
#5081,#5082,#5083,#5084),.UNSPECIFIED.,.F.,.F.,(4,2,2,2,4),(0.941657228299604,
1.01969462928961,1.09773203027962,1.17663750067288,1.25554297106614),
 .UNSPECIFIED.);
#267=B_SPLINE_CURVE_WITH_KNOTS('',3,(#5088,#5089,#5090,#5091,#5092,#5093,
#5094,#5095,#5096,#5097,#5098,#5099,#5100,#5101,#5102,#5103,#5104,#5105),
 .UNSPECIFIED.,.F.,.F.,(4,2,2,2,2,2,2,2,4),(0.313885742766534,0.391923143756543,
0.469960544746551,0.54886601513981,0.627771485533069,0.706676955926329,
0.785582426319588,0.863619827309596,0.941657228299604),.UNSPECIFIED.);
#268=B_SPLINE_CURVE_WITH_KNOTS('',3,(#5137,#5138,#5139,#5140,#5141,#5142,
#5143,#5144,#5145,#5146),.UNSPECIFIED.,.F.,.F.,(4,2,2,2,4),(0.,0.0789054703932594,
0.157810940786519,0.235848341776527,0.313885742766535),.UNSPECIFIED.);
#269=B_SPLINE_CURVE_WITH_KNOTS('',3,(#5148,#5149,#5150,#5151,#5152,#5153,
#5154,#5155,#5156,#5157),.UNSPECIFIED.,.F.,.F.,(4,2,2,2,4),(0.941657228299605,
1.01969462928961,1.09773203027962,1.17663750067288,1.25554297106614),
 .UNSPECIFIED.);
#270=B_SPLINE_CURVE_WITH_KNOTS('',3,(#5161,#5162,#5163,#5164,#5165,#5166,
#5167,#5168,#5169,#5170,#5171,#5172,#5173,#5174,#5175,#5176,#5177,#5178),
 .UNSPECIFIED.,.F.,.F.,(4,2,2,2,2,2,2,2,4),(0.313885742766535,0.391923143756543,
0.469960544746551,0.54886601513981,0.62777148553307,0.706676955926329,0.785582426319589,
0.863619827309597,0.941657228299605),.UNSPECIFIED.);
#271=B_SPLINE_CURVE_WITH_KNOTS('',3,(#5182,#5183,#5184,#5185,#5186,#5187,
#5188,#5189,#5190,#5191),.UNSPECIFIED.,.F.,.F.,(4,2,2,2,4),(0.,0.0789054703932594,
0.157810940786519,0.235848341776527,0.313885742766535),.UNSPECIFIED.);
#272=B_SPLINE_CURVE_WITH_KNOTS('',3,(#5193,#5194,#5195,#5196,#5197,#5198,
#5199,#5200,#5201,#5202),.UNSPECIFIED.,.F.,.F.,(4,2,2,2,4),(0.941657228299605,
1.01969462928961,1.09773203027962,1.17663750067288,1.25554297106614),
 .UNSPECIFIED.);
#273=B_SPLINE_CURVE_WITH_KNOTS('',3,(#5206,#5207,#5208,#5209,#5210,#5211,
#5212,#5213,#5214,#5215,#5216,#5217,#5218,#5219,#5220,#5221,#5222,#5223),
 .UNSPECIFIED.,.F.,.F.,(4,2,2,2,2,2,2,2,4),(0.313885742766535,0.391923143756543,
0.469960544746551,0.548866015139811,0.62777148553307,0.706676955926329,
0.785582426319589,0.863619827309597,0.941657228299605),.UNSPECIFIED.);
#274=B_SPLINE_CURVE_WITH_KNOTS('',3,(#5227,#5228,#5229,#5230,#5231,#5232,
#5233,#5234,#5235,#5236),.UNSPECIFIED.,.F.,.F.,(4,2,2,2,4),(0.,0.0789054703932594,
0.157810940786519,0.235848341776527,0.313885742766535),.UNSPECIFIED.);
#275=B_SPLINE_CURVE_WITH_KNOTS('',3,(#5238,#5239,#5240,#5241,#5242,#5243,
#5244,#5245,#5246,#5247),.UNSPECIFIED.,.F.,.F.,(4,2,2,2,4),(0.941657228299605,
1.01969462928961,1.09773203027962,1.17663750067288,1.25554297106614),
 .UNSPECIFIED.);
#276=B_SPLINE_CURVE_WITH_KNOTS('',3,(#5251,#5252,#5253,#5254,#5255,#5256,
#5257,#5258,#5259,#5260,#5261,#5262,#5263,#5264,#5265,#5266,#5267,#5268),
 .UNSPECIFIED.,.F.,.F.,(4,2,2,2,2,2,2,2,4),(0.313885742766535,0.391923143756543,
0.469960544746551,0.54886601513981,0.62777148553307,0.706676955926329,0.785582426319589,
0.863619827309597,0.941657228299605),.UNSPECIFIED.);
#277=PLANE('',#3509);
#278=PLANE('',#3513);
#279=PLANE('',#3517);
#280=PLANE('',#3521);
#281=PLANE('',#3531);
#282=PLANE('',#3535);
#283=PLANE('',#3539);
#284=PLANE('',#3543);
#285=PLANE('',#3565);
#286=PLANE('',#3570);
#287=PLANE('',#3575);
#288=PLANE('',#3580);
#289=PLANE('',#3585);
#290=PLANE('',#3590);
#291=PLANE('',#3595);
#292=PLANE('',#3596);
#293=PLANE('',#3597);
#294=PLANE('',#3598);
#295=PLANE('',#3599);
#296=PLANE('',#3600);
#297=PLANE('',#3620);
#298=PLANE('',#3622);
#299=PLANE('',#3627);
#300=PLANE('',#3635);
#301=PLANE('',#3636);
#302=PLANE('',#3656);
#303=PLANE('',#3658);
#304=PLANE('',#3663);
#305=PLANE('',#3671);
#306=PLANE('',#3672);
#307=PLANE('',#3674);
#308=PLANE('',#3676);
#309=PLANE('',#3678);
#310=PLANE('',#3679);
#311=PLANE('',#3680);
#312=PLANE('',#3681);
#313=PLANE('',#3682);
#314=PLANE('',#3683);
#315=PLANE('',#3686);
#316=PLANE('',#3694);
#317=PLANE('',#3698);
#318=PLANE('',#3700);
#319=PLANE('',#3701);
#320=PLANE('',#3702);
#321=PLANE('',#3703);
#322=PLANE('',#3704);
#323=PLANE('',#3705);
#324=PLANE('',#3706);
#325=PLANE('',#3709);
#326=PLANE('',#3711);
#327=PLANE('',#3712);
#328=PLANE('',#3713);
#329=PLANE('',#3714);
#330=PLANE('',#3715);
#331=PLANE('',#3716);
#332=PLANE('',#3720);
#333=PLANE('',#3726);
#334=PLANE('',#3731);
#335=PLANE('',#3736);
#336=PLANE('',#3741);
#337=PLANE('',#3754);
#338=PLANE('',#3764);
#339=PLANE('',#3765);
#340=PLANE('',#3766);
#341=PLANE('',#3767);
#342=PLANE('',#3768);
#343=PLANE('',#3769);
#344=PLANE('',#3792);
#345=PLANE('',#3793);
#346=PLANE('',#3794);
#347=PLANE('',#3795);
#348=PLANE('',#3796);
#349=PLANE('',#3797);
#350=PLANE('',#3802);
#351=PLANE('',#3804);
#352=PLANE('',#3806);
#353=PLANE('',#3807);
#354=PLANE('',#3808);
#355=PLANE('',#3809);
#356=PLANE('',#3810);
#357=PLANE('',#3811);
#358=PLANE('',#3812);
#359=PLANE('',#3817);
#360=PLANE('',#3823);
#361=PLANE('',#3825);
#362=PLANE('',#3827);
#363=PLANE('',#3829);
#364=PLANE('',#3830);
#365=PLANE('',#3831);
#366=PLANE('',#3832);
#367=PLANE('',#3833);
#368=PLANE('',#3834);
#369=PLANE('',#3835);
#370=PLANE('',#3839);
#371=PLANE('',#3844);
#372=PLANE('',#3848);
#373=PLANE('',#3853);
#374=PLANE('',#3857);
#375=PLANE('',#3863);
#376=PLANE('',#3871);
#377=PLANE('',#3879);
#378=PLANE('',#3880);
#379=PLANE('',#3881);
#380=PLANE('',#3882);
#381=PLANE('',#3883);
#382=PLANE('',#3884);
#383=PLANE('',#3885);
#384=PLANE('',#3886);
#385=PLANE('',#3887);
#386=FACE_OUTER_BOUND('',#585,.T.);
#387=FACE_OUTER_BOUND('',#586,.T.);
#388=FACE_OUTER_BOUND('',#587,.T.);
#389=FACE_OUTER_BOUND('',#588,.T.);
#390=FACE_OUTER_BOUND('',#589,.T.);
#391=FACE_OUTER_BOUND('',#590,.T.);
#392=FACE_OUTER_BOUND('',#591,.T.);
#393=FACE_OUTER_BOUND('',#592,.T.);
#394=FACE_OUTER_BOUND('',#593,.T.);
#395=FACE_OUTER_BOUND('',#594,.T.);
#396=FACE_OUTER_BOUND('',#595,.T.);
#397=FACE_OUTER_BOUND('',#596,.T.);
#398=FACE_OUTER_BOUND('',#597,.T.);
#399=FACE_OUTER_BOUND('',#598,.T.);
#400=FACE_OUTER_BOUND('',#599,.T.);
#401=FACE_OUTER_BOUND('',#600,.T.);
#402=FACE_OUTER_BOUND('',#601,.T.);
#403=FACE_OUTER_BOUND('',#602,.T.);
#404=FACE_OUTER_BOUND('',#603,.T.);
#405=FACE_OUTER_BOUND('',#604,.T.);
#406=FACE_OUTER_BOUND('',#605,.T.);
#407=FACE_OUTER_BOUND('',#606,.T.);
#408=FACE_OUTER_BOUND('',#607,.T.);
#409=FACE_OUTER_BOUND('',#608,.T.);
#410=FACE_OUTER_BOUND('',#609,.T.);
#411=FACE_OUTER_BOUND('',#610,.T.);
#412=FACE_OUTER_BOUND('',#611,.T.);
#413=FACE_OUTER_BOUND('',#612,.T.);
#414=FACE_OUTER_BOUND('',#614,.T.);
#415=FACE_OUTER_BOUND('',#615,.T.);
#416=FACE_OUTER_BOUND('',#617,.T.);
#417=FACE_OUTER_BOUND('',#618,.T.);
#418=FACE_OUTER_BOUND('',#620,.T.);
#419=FACE_OUTER_BOUND('',#621,.T.);
#420=FACE_OUTER_BOUND('',#623,.T.);
#421=FACE_OUTER_BOUND('',#624,.T.);
#422=FACE_OUTER_BOUND('',#626,.T.);
#423=FACE_OUTER_BOUND('',#627,.T.);
#424=FACE_OUTER_BOUND('',#629,.T.);
#425=FACE_OUTER_BOUND('',#630,.T.);
#426=FACE_OUTER_BOUND('',#631,.T.);
#427=FACE_OUTER_BOUND('',#632,.T.);
#428=FACE_OUTER_BOUND('',#633,.T.);
#429=FACE_OUTER_BOUND('',#637,.T.);
#430=FACE_OUTER_BOUND('',#638,.T.);
#431=FACE_OUTER_BOUND('',#642,.T.);
#432=FACE_OUTER_BOUND('',#661,.T.);
#433=FACE_OUTER_BOUND('',#666,.T.);
#434=FACE_OUTER_BOUND('',#667,.T.);
#435=FACE_OUTER_BOUND('',#668,.T.);
#436=FACE_OUTER_BOUND('',#669,.T.);
#437=FACE_OUTER_BOUND('',#670,.T.);
#438=FACE_OUTER_BOUND('',#671,.T.);
#439=FACE_OUTER_BOUND('',#672,.T.);
#440=FACE_OUTER_BOUND('',#679,.T.);
#441=FACE_OUTER_BOUND('',#681,.T.);
#442=FACE_OUTER_BOUND('',#682,.T.);
#443=FACE_OUTER_BOUND('',#689,.T.);
#444=FACE_OUTER_BOUND('',#690,.T.);
#445=FACE_OUTER_BOUND('',#691,.T.);
#446=FACE_OUTER_BOUND('',#692,.T.);
#447=FACE_OUTER_BOUND('',#694,.T.);
#448=FACE_OUTER_BOUND('',#696,.T.);
#449=FACE_OUTER_BOUND('',#697,.T.);
#450=FACE_OUTER_BOUND('',#698,.T.);
#451=FACE_OUTER_BOUND('',#699,.T.);
#452=FACE_OUTER_BOUND('',#700,.T.);
#453=FACE_OUTER_BOUND('',#701,.T.);
#454=FACE_OUTER_BOUND('',#702,.T.);
#455=FACE_OUTER_BOUND('',#709,.T.);
#456=FACE_OUTER_BOUND('',#711,.T.);
#457=FACE_OUTER_BOUND('',#712,.T.);
#458=FACE_OUTER_BOUND('',#719,.T.);
#459=FACE_OUTER_BOUND('',#720,.T.);
#460=FACE_OUTER_BOUND('',#721,.T.);
#461=FACE_OUTER_BOUND('',#722,.T.);
#462=FACE_OUTER_BOUND('',#724,.T.);
#463=FACE_OUTER_BOUND('',#726,.T.);
#464=FACE_OUTER_BOUND('',#728,.T.);
#465=FACE_OUTER_BOUND('',#730,.T.);
#466=FACE_OUTER_BOUND('',#731,.T.);
#467=FACE_OUTER_BOUND('',#732,.T.);
#468=FACE_OUTER_BOUND('',#733,.T.);
#469=FACE_OUTER_BOUND('',#734,.T.);
#470=FACE_OUTER_BOUND('',#735,.T.);
#471=FACE_OUTER_BOUND('',#736,.T.);
#472=FACE_OUTER_BOUND('',#737,.T.);
#473=FACE_OUTER_BOUND('',#739,.T.);
#474=FACE_OUTER_BOUND('',#740,.T.);
#475=FACE_OUTER_BOUND('',#741,.T.);
#476=FACE_OUTER_BOUND('',#742,.T.);
#477=FACE_OUTER_BOUND('',#744,.T.);
#478=FACE_OUTER_BOUND('',#745,.T.);
#479=FACE_OUTER_BOUND('',#747,.T.);
#480=FACE_OUTER_BOUND('',#748,.T.);
#481=FACE_OUTER_BOUND('',#749,.T.);
#482=FACE_OUTER_BOUND('',#750,.T.);
#483=FACE_OUTER_BOUND('',#751,.T.);
#484=FACE_OUTER_BOUND('',#752,.T.);
#485=FACE_OUTER_BOUND('',#753,.T.);
#486=FACE_OUTER_BOUND('',#754,.T.);
#487=FACE_OUTER_BOUND('',#755,.T.);
#488=FACE_OUTER_BOUND('',#756,.T.);
#489=FACE_OUTER_BOUND('',#757,.T.);
#490=FACE_OUTER_BOUND('',#758,.T.);
#491=FACE_OUTER_BOUND('',#759,.T.);
#492=FACE_OUTER_BOUND('',#760,.T.);
#493=FACE_OUTER_BOUND('',#761,.T.);
#494=FACE_OUTER_BOUND('',#763,.T.);
#495=FACE_OUTER_BOUND('',#764,.T.);
#496=FACE_OUTER_BOUND('',#765,.T.);
#497=FACE_OUTER_BOUND('',#766,.T.);
#498=FACE_OUTER_BOUND('',#768,.T.);
#499=FACE_OUTER_BOUND('',#769,.T.);
#500=FACE_OUTER_BOUND('',#771,.T.);
#501=FACE_OUTER_BOUND('',#772,.T.);
#502=FACE_OUTER_BOUND('',#774,.T.);
#503=FACE_OUTER_BOUND('',#775,.T.);
#504=FACE_OUTER_BOUND('',#777,.T.);
#505=FACE_OUTER_BOUND('',#778,.T.);
#506=FACE_OUTER_BOUND('',#779,.T.);
#507=FACE_OUTER_BOUND('',#780,.T.);
#508=FACE_OUTER_BOUND('',#781,.T.);
#509=FACE_OUTER_BOUND('',#782,.T.);
#510=FACE_OUTER_BOUND('',#784,.T.);
#511=FACE_OUTER_BOUND('',#785,.T.);
#512=FACE_OUTER_BOUND('',#786,.T.);
#513=FACE_OUTER_BOUND('',#787,.T.);
#514=FACE_OUTER_BOUND('',#788,.T.);
#515=FACE_OUTER_BOUND('',#789,.T.);
#516=FACE_OUTER_BOUND('',#790,.T.);
#517=FACE_OUTER_BOUND('',#791,.T.);
#518=FACE_OUTER_BOUND('',#799,.T.);
#519=FACE_OUTER_BOUND('',#807,.T.);
#520=FACE_OUTER_BOUND('',#808,.T.);
#521=FACE_OUTER_BOUND('',#809,.T.);
#522=FACE_OUTER_BOUND('',#810,.T.);
#523=FACE_OUTER_BOUND('',#811,.T.);
#524=FACE_OUTER_BOUND('',#812,.T.);
#525=FACE_OUTER_BOUND('',#813,.T.);
#526=FACE_OUTER_BOUND('',#814,.T.);
#527=FACE_OUTER_BOUND('',#815,.T.);
#528=FACE_OUTER_BOUND('',#816,.T.);
#529=FACE_OUTER_BOUND('',#817,.T.);
#530=FACE_OUTER_BOUND('',#818,.T.);
#531=FACE_OUTER_BOUND('',#826,.T.);
#532=FACE_OUTER_BOUND('',#834,.T.);
#533=FACE_OUTER_BOUND('',#835,.T.);
#534=FACE_OUTER_BOUND('',#837,.T.);
#535=FACE_OUTER_BOUND('',#839,.T.);
#536=FACE_OUTER_BOUND('',#840,.T.);
#537=FACE_OUTER_BOUND('',#841,.T.);
#538=FACE_OUTER_BOUND('',#842,.T.);
#539=FACE_OUTER_BOUND('',#843,.T.);
#540=FACE_OUTER_BOUND('',#844,.T.);
#541=FACE_OUTER_BOUND('',#845,.T.);
#542=FACE_OUTER_BOUND('',#847,.T.);
#543=FACE_OUTER_BOUND('',#848,.T.);
#544=FACE_OUTER_BOUND('',#849,.T.);
#545=FACE_OUTER_BOUND('',#851,.T.);
#546=FACE_OUTER_BOUND('',#852,.T.);
#547=FACE_OUTER_BOUND('',#854,.T.);
#548=FACE_OUTER_BOUND('',#856,.T.);
#549=FACE_OUTER_BOUND('',#858,.T.);
#550=FACE_OUTER_BOUND('',#859,.T.);
#551=FACE_OUTER_BOUND('',#860,.T.);
#552=FACE_OUTER_BOUND('',#861,.T.);
#553=FACE_OUTER_BOUND('',#862,.T.);
#554=FACE_OUTER_BOUND('',#863,.T.);
#555=FACE_OUTER_BOUND('',#864,.T.);
#556=FACE_OUTER_BOUND('',#866,.T.);
#557=FACE_OUTER_BOUND('',#867,.T.);
#558=FACE_OUTER_BOUND('',#869,.T.);
#559=FACE_OUTER_BOUND('',#870,.T.);
#560=FACE_OUTER_BOUND('',#871,.T.);
#561=FACE_OUTER_BOUND('',#873,.T.);
#562=FACE_OUTER_BOUND('',#874,.T.);
#563=FACE_OUTER_BOUND('',#876,.T.);
#564=FACE_OUTER_BOUND('',#877,.T.);
#565=FACE_OUTER_BOUND('',#879,.T.);
#566=FACE_OUTER_BOUND('',#880,.T.);
#567=FACE_OUTER_BOUND('',#882,.T.);
#568=FACE_OUTER_BOUND('',#883,.T.);
#569=FACE_OUTER_BOUND('',#884,.T.);
#570=FACE_OUTER_BOUND('',#885,.T.);
#571=FACE_OUTER_BOUND('',#886,.T.);
#572=FACE_OUTER_BOUND('',#887,.T.);
#573=FACE_OUTER_BOUND('',#889,.T.);
#574=FACE_OUTER_BOUND('',#890,.T.);
#575=FACE_OUTER_BOUND('',#891,.T.);
#576=FACE_OUTER_BOUND('',#892,.T.);
#577=FACE_OUTER_BOUND('',#893,.T.);
#578=FACE_OUTER_BOUND('',#894,.T.);
#579=FACE_OUTER_BOUND('',#895,.T.);
#580=FACE_OUTER_BOUND('',#896,.T.);
#581=FACE_OUTER_BOUND('',#897,.T.);
#582=FACE_OUTER_BOUND('',#898,.T.);
#583=FACE_OUTER_BOUND('',#899,.T.);
#584=FACE_OUTER_BOUND('',#900,.T.);
#585=EDGE_LOOP('',(#2235,#2236,#2237,#2238));
#586=EDGE_LOOP('',(#2239));
#587=EDGE_LOOP('',(#2240,#2241,#2242,#2243));
#588=EDGE_LOOP('',(#2244));
#589=EDGE_LOOP('',(#2245,#2246,#2247,#2248));
#590=EDGE_LOOP('',(#2249));
#591=EDGE_LOOP('',(#2250,#2251,#2252,#2253));
#592=EDGE_LOOP('',(#2254));
#593=EDGE_LOOP('',(#2255,#2256,#2257,#2258,#2259,#2260));
#594=EDGE_LOOP('',(#2261,#2262,#2263,#2264,#2265,#2266));
#595=EDGE_LOOP('',(#2267,#2268,#2269,#2270,#2271,#2272));
#596=EDGE_LOOP('',(#2273,#2274,#2275,#2276));
#597=EDGE_LOOP('',(#2277));
#598=EDGE_LOOP('',(#2278,#2279,#2280,#2281));
#599=EDGE_LOOP('',(#2282));
#600=EDGE_LOOP('',(#2283,#2284,#2285,#2286));
#601=EDGE_LOOP('',(#2287));
#602=EDGE_LOOP('',(#2288,#2289,#2290,#2291));
#603=EDGE_LOOP('',(#2292));
#604=EDGE_LOOP('',(#2293,#2294,#2295,#2296,#2297,#2298));
#605=EDGE_LOOP('',(#2299,#2300,#2301,#2302,#2303,#2304));
#606=EDGE_LOOP('',(#2305,#2306,#2307,#2308,#2309,#2310));
#607=EDGE_LOOP('',(#2311,#2312,#2313,#2314));
#608=EDGE_LOOP('',(#2315,#2316,#2317,#2318));
#609=EDGE_LOOP('',(#2319,#2320,#2321,#2322));
#610=EDGE_LOOP('',(#2323,#2324,#2325,#2326));
#611=EDGE_LOOP('',(#2327,#2328,#2329,#2330));
#612=EDGE_LOOP('',(#2331));
#613=EDGE_LOOP('',(#2332));
#614=EDGE_LOOP('',(#2333,#2334,#2335,#2336));
#615=EDGE_LOOP('',(#2337));
#616=EDGE_LOOP('',(#2338));
#617=EDGE_LOOP('',(#2339,#2340,#2341,#2342));
#618=EDGE_LOOP('',(#2343));
#619=EDGE_LOOP('',(#2344));
#620=EDGE_LOOP('',(#2345,#2346,#2347,#2348));
#621=EDGE_LOOP('',(#2349));
#622=EDGE_LOOP('',(#2350));
#623=EDGE_LOOP('',(#2351,#2352,#2353,#2354));
#624=EDGE_LOOP('',(#2355));
#625=EDGE_LOOP('',(#2356));
#626=EDGE_LOOP('',(#2357,#2358,#2359,#2360));
#627=EDGE_LOOP('',(#2361));
#628=EDGE_LOOP('',(#2362));
#629=EDGE_LOOP('',(#2363,#2364,#2365,#2366,#2367,#2368,#2369,#2370,#2371,
#2372,#2373,#2374,#2375,#2376));
#630=EDGE_LOOP('',(#2377,#2378,#2379,#2380,#2381,#2382,#2383,#2384,#2385,
#2386,#2387,#2388,#2389,#2390));
#631=EDGE_LOOP('',(#2391,#2392,#2393,#2394,#2395,#2396,#2397,#2398,#2399,
#2400,#2401,#2402,#2403,#2404));
#632=EDGE_LOOP('',(#2405,#2406,#2407,#2408));
#633=EDGE_LOOP('',(#2409,#2410,#2411,#2412));
#634=EDGE_LOOP('',(#2413));
#635=EDGE_LOOP('',(#2414));
#636=EDGE_LOOP('',(#2415));
#637=EDGE_LOOP('',(#2416,#2417,#2418,#2419));
#638=EDGE_LOOP('',(#2420,#2421,#2422,#2423));
#639=EDGE_LOOP('',(#2424));
#640=EDGE_LOOP('',(#2425));
#641=EDGE_LOOP('',(#2426));
#642=EDGE_LOOP('',(#2427,#2428,#2429,#2430));
#643=EDGE_LOOP('',(#2431));
#644=EDGE_LOOP('',(#2432));
#645=EDGE_LOOP('',(#2433));
#646=EDGE_LOOP('',(#2434));
#647=EDGE_LOOP('',(#2435));
#648=EDGE_LOOP('',(#2436));
#649=EDGE_LOOP('',(#2437));
#650=EDGE_LOOP('',(#2438));
#651=EDGE_LOOP('',(#2439));
#652=EDGE_LOOP('',(#2440));
#653=EDGE_LOOP('',(#2441));
#654=EDGE_LOOP('',(#2442));
#655=EDGE_LOOP('',(#2443));
#656=EDGE_LOOP('',(#2444));
#657=EDGE_LOOP('',(#2445));
#658=EDGE_LOOP('',(#2446));
#659=EDGE_LOOP('',(#2447));
#660=EDGE_LOOP('',(#2448));
#661=EDGE_LOOP('',(#2449,#2450,#2451,#2452));
#662=EDGE_LOOP('',(#2453));
#663=EDGE_LOOP('',(#2454));
#664=EDGE_LOOP('',(#2455));
#665=EDGE_LOOP('',(#2456));
#666=EDGE_LOOP('',(#2457,#2458,#2459,#2460));
#667=EDGE_LOOP('',(#2461,#2462,#2463,#2464));
#668=EDGE_LOOP('',(#2465,#2466,#2467,#2468));
#669=EDGE_LOOP('',(#2469,#2470,#2471,#2472));
#670=EDGE_LOOP('',(#2473,#2474,#2475,#2476));
#671=EDGE_LOOP('',(#2477,#2478,#2479,#2480));
#672=EDGE_LOOP('',(#2481));
#673=EDGE_LOOP('',(#2482));
#674=EDGE_LOOP('',(#2483));
#675=EDGE_LOOP('',(#2484));
#676=EDGE_LOOP('',(#2485));
#677=EDGE_LOOP('',(#2486));
#678=EDGE_LOOP('',(#2487));
#679=EDGE_LOOP('',(#2488));
#680=EDGE_LOOP('',(#2489));
#681=EDGE_LOOP('',(#2490,#2491,#2492,#2493));
#682=EDGE_LOOP('',(#2494));
#683=EDGE_LOOP('',(#2495));
#684=EDGE_LOOP('',(#2496));
#685=EDGE_LOOP('',(#2497));
#686=EDGE_LOOP('',(#2498));
#687=EDGE_LOOP('',(#2499));
#688=EDGE_LOOP('',(#2500));
#689=EDGE_LOOP('',(#2501,#2502,#2503,#2504));
#690=EDGE_LOOP('',(#2505,#2506,#2507,#2508));
#691=EDGE_LOOP('',(#2509,#2510,#2511,#2512));
#692=EDGE_LOOP('',(#2513));
#693=EDGE_LOOP('',(#2514));
#694=EDGE_LOOP('',(#2515));
#695=EDGE_LOOP('',(#2516));
#696=EDGE_LOOP('',(#2517,#2518,#2519,#2520));
#697=EDGE_LOOP('',(#2521,#2522,#2523,#2524));
#698=EDGE_LOOP('',(#2525,#2526,#2527,#2528));
#699=EDGE_LOOP('',(#2529,#2530,#2531,#2532));
#700=EDGE_LOOP('',(#2533,#2534,#2535,#2536));
#701=EDGE_LOOP('',(#2537,#2538,#2539,#2540));
#702=EDGE_LOOP('',(#2541));
#703=EDGE_LOOP('',(#2542));
#704=EDGE_LOOP('',(#2543));
#705=EDGE_LOOP('',(#2544));
#706=EDGE_LOOP('',(#2545));
#707=EDGE_LOOP('',(#2546));
#708=EDGE_LOOP('',(#2547));
#709=EDGE_LOOP('',(#2548));
#710=EDGE_LOOP('',(#2549));
#711=EDGE_LOOP('',(#2550,#2551,#2552,#2553));
#712=EDGE_LOOP('',(#2554));
#713=EDGE_LOOP('',(#2555));
#714=EDGE_LOOP('',(#2556));
#715=EDGE_LOOP('',(#2557));
#716=EDGE_LOOP('',(#2558));
#717=EDGE_LOOP('',(#2559));
#718=EDGE_LOOP('',(#2560));
#719=EDGE_LOOP('',(#2561,#2562,#2563,#2564));
#720=EDGE_LOOP('',(#2565,#2566,#2567,#2568));
#721=EDGE_LOOP('',(#2569,#2570,#2571,#2572));
#722=EDGE_LOOP('',(#2573));
#723=EDGE_LOOP('',(#2574));
#724=EDGE_LOOP('',(#2575));
#725=EDGE_LOOP('',(#2576));
#726=EDGE_LOOP('',(#2577,#2578,#2579,#2580,#2581,#2582));
#727=EDGE_LOOP('',(#2583));
#728=EDGE_LOOP('',(#2584,#2585,#2586,#2587,#2588,#2589));
#729=EDGE_LOOP('',(#2590));
#730=EDGE_LOOP('',(#2591,#2592,#2593,#2594));
#731=EDGE_LOOP('',(#2595,#2596,#2597,#2598));
#732=EDGE_LOOP('',(#2599,#2600,#2601,#2602));
#733=EDGE_LOOP('',(#2603,#2604,#2605,#2606));
#734=EDGE_LOOP('',(#2607,#2608,#2609,#2610));
#735=EDGE_LOOP('',(#2611,#2612,#2613,#2614));
#736=EDGE_LOOP('',(#2615,#2616,#2617,#2618));
#737=EDGE_LOOP('',(#2619));
#738=EDGE_LOOP('',(#2620));
#739=EDGE_LOOP('',(#2621,#2622,#2623,#2624));
#740=EDGE_LOOP('',(#2625,#2626,#2627,#2628));
#741=EDGE_LOOP('',(#2629,#2630,#2631,#2632));
#742=EDGE_LOOP('',(#2633));
#743=EDGE_LOOP('',(#2634));
#744=EDGE_LOOP('',(#2635,#2636,#2637,#2638));
#745=EDGE_LOOP('',(#2639,#2640,#2641,#2642,#2643,#2644));
#746=EDGE_LOOP('',(#2645));
#747=EDGE_LOOP('',(#2646,#2647,#2648,#2649));
#748=EDGE_LOOP('',(#2650,#2651,#2652,#2653));
#749=EDGE_LOOP('',(#2654,#2655,#2656,#2657));
#750=EDGE_LOOP('',(#2658,#2659,#2660,#2661));
#751=EDGE_LOOP('',(#2662,#2663,#2664,#2665));
#752=EDGE_LOOP('',(#2666,#2667,#2668,#2669));
#753=EDGE_LOOP('',(#2670,#2671,#2672,#2673,#2674,#2675));
#754=EDGE_LOOP('',(#2676,#2677,#2678,#2679));
#755=EDGE_LOOP('',(#2680));
#756=EDGE_LOOP('',(#2681,#2682,#2683,#2684));
#757=EDGE_LOOP('',(#2685,#2686,#2687,#2688));
#758=EDGE_LOOP('',(#2689,#2690,#2691,#2692));
#759=EDGE_LOOP('',(#2693,#2694,#2695,#2696));
#760=EDGE_LOOP('',(#2697,#2698,#2699,#2700));
#761=EDGE_LOOP('',(#2701));
#762=EDGE_LOOP('',(#2702,#2703,#2704,#2705));
#763=EDGE_LOOP('',(#2706,#2707,#2708,#2709));
#764=EDGE_LOOP('',(#2710));
#765=EDGE_LOOP('',(#2711,#2712,#2713,#2714));
#766=EDGE_LOOP('',(#2715));
#767=EDGE_LOOP('',(#2716));
#768=EDGE_LOOP('',(#2717,#2718,#2719,#2720));
#769=EDGE_LOOP('',(#2721));
#770=EDGE_LOOP('',(#2722));
#771=EDGE_LOOP('',(#2723,#2724,#2725,#2726));
#772=EDGE_LOOP('',(#2727));
#773=EDGE_LOOP('',(#2728));
#774=EDGE_LOOP('',(#2729,#2730,#2731,#2732));
#775=EDGE_LOOP('',(#2733));
#776=EDGE_LOOP('',(#2734));
#777=EDGE_LOOP('',(#2735,#2736,#2737,#2738));
#778=EDGE_LOOP('',(#2739,#2740,#2741,#2742));
#779=EDGE_LOOP('',(#2743,#2744,#2745,#2746));
#780=EDGE_LOOP('',(#2747,#2748,#2749,#2750));
#781=EDGE_LOOP('',(#2751,#2752,#2753,#2754));
#782=EDGE_LOOP('',(#2755));
#783=EDGE_LOOP('',(#2756));
#784=EDGE_LOOP('',(#2757,#2758,#2759,#2760));
#785=EDGE_LOOP('',(#2761,#2762,#2763,#2764));
#786=EDGE_LOOP('',(#2765,#2766,#2767,#2768));
#787=EDGE_LOOP('',(#2769,#2770,#2771,#2772));
#788=EDGE_LOOP('',(#2773,#2774,#2775,#2776));
#789=EDGE_LOOP('',(#2777,#2778,#2779,#2780));
#790=EDGE_LOOP('',(#2781,#2782,#2783,#2784));
#791=EDGE_LOOP('',(#2785,#2786,#2787,#2788));
#792=EDGE_LOOP('',(#2789));
#793=EDGE_LOOP('',(#2790));
#794=EDGE_LOOP('',(#2791));
#795=EDGE_LOOP('',(#2792));
#796=EDGE_LOOP('',(#2793));
#797=EDGE_LOOP('',(#2794));
#798=EDGE_LOOP('',(#2795));
#799=EDGE_LOOP('',(#2796,#2797,#2798,#2799));
#800=EDGE_LOOP('',(#2800));
#801=EDGE_LOOP('',(#2801));
#802=EDGE_LOOP('',(#2802));
#803=EDGE_LOOP('',(#2803));
#804=EDGE_LOOP('',(#2804));
#805=EDGE_LOOP('',(#2805));
#806=EDGE_LOOP('',(#2806));
#807=EDGE_LOOP('',(#2807,#2808,#2809,#2810));
#808=EDGE_LOOP('',(#2811,#2812,#2813,#2814));
#809=EDGE_LOOP('',(#2815,#2816,#2817,#2818));
#810=EDGE_LOOP('',(#2819,#2820,#2821,#2822));
#811=EDGE_LOOP('',(#2823,#2824,#2825,#2826));
#812=EDGE_LOOP('',(#2827,#2828,#2829,#2830));
#813=EDGE_LOOP('',(#2831,#2832,#2833,#2834));
#814=EDGE_LOOP('',(#2835,#2836,#2837,#2838));
#815=EDGE_LOOP('',(#2839,#2840,#2841,#2842));
#816=EDGE_LOOP('',(#2843,#2844,#2845,#2846));
#817=EDGE_LOOP('',(#2847,#2848,#2849,#2850));
#818=EDGE_LOOP('',(#2851,#2852,#2853,#2854));
#819=EDGE_LOOP('',(#2855));
#820=EDGE_LOOP('',(#2856));
#821=EDGE_LOOP('',(#2857));
#822=EDGE_LOOP('',(#2858));
#823=EDGE_LOOP('',(#2859));
#824=EDGE_LOOP('',(#2860));
#825=EDGE_LOOP('',(#2861));
#826=EDGE_LOOP('',(#2862,#2863,#2864,#2865));
#827=EDGE_LOOP('',(#2866));
#828=EDGE_LOOP('',(#2867));
#829=EDGE_LOOP('',(#2868));
#830=EDGE_LOOP('',(#2869));
#831=EDGE_LOOP('',(#2870));
#832=EDGE_LOOP('',(#2871));
#833=EDGE_LOOP('',(#2872));
#834=EDGE_LOOP('',(#2873,#2874,#2875,#2876));
#835=EDGE_LOOP('',(#2877));
#836=EDGE_LOOP('',(#2878));
#837=EDGE_LOOP('',(#2879,#2880,#2881,#2882,#2883,#2884));
#838=EDGE_LOOP('',(#2885));
#839=EDGE_LOOP('',(#2886,#2887,#2888,#2889));
#840=EDGE_LOOP('',(#2890,#2891,#2892,#2893));
#841=EDGE_LOOP('',(#2894,#2895,#2896,#2897));
#842=EDGE_LOOP('',(#2898,#2899,#2900,#2901));
#843=EDGE_LOOP('',(#2902,#2903,#2904,#2905));
#844=EDGE_LOOP('',(#2906,#2907,#2908,#2909));
#845=EDGE_LOOP('',(#2910,#2911,#2912,#2913,#2914,#2915));
#846=EDGE_LOOP('',(#2916));
#847=EDGE_LOOP('',(#2917,#2918,#2919,#2920));
#848=EDGE_LOOP('',(#2921,#2922,#2923,#2924));
#849=EDGE_LOOP('',(#2925));
#850=EDGE_LOOP('',(#2926));
#851=EDGE_LOOP('',(#2927,#2928,#2929,#2930));
#852=EDGE_LOOP('',(#2931));
#853=EDGE_LOOP('',(#2932));
#854=EDGE_LOOP('',(#2933,#2934,#2935,#2936,#2937,#2938));
#855=EDGE_LOOP('',(#2939));
#856=EDGE_LOOP('',(#2940,#2941,#2942,#2943,#2944,#2945));
#857=EDGE_LOOP('',(#2946));
#858=EDGE_LOOP('',(#2947,#2948,#2949,#2950));
#859=EDGE_LOOP('',(#2951,#2952,#2953,#2954));
#860=EDGE_LOOP('',(#2955,#2956,#2957,#2958));
#861=EDGE_LOOP('',(#2959,#2960,#2961,#2962));
#862=EDGE_LOOP('',(#2963,#2964,#2965,#2966));
#863=EDGE_LOOP('',(#2967,#2968,#2969,#2970));
#864=EDGE_LOOP('',(#2971));
#865=EDGE_LOOP('',(#2972));
#866=EDGE_LOOP('',(#2973,#2974,#2975,#2976));
#867=EDGE_LOOP('',(#2977));
#868=EDGE_LOOP('',(#2978));
#869=EDGE_LOOP('',(#2979,#2980,#2981,#2982));
#870=EDGE_LOOP('',(#2983,#2984,#2985,#2986));
#871=EDGE_LOOP('',(#2987));
#872=EDGE_LOOP('',(#2988));
#873=EDGE_LOOP('',(#2989,#2990,#2991,#2992));
#874=EDGE_LOOP('',(#2993));
#875=EDGE_LOOP('',(#2994));
#876=EDGE_LOOP('',(#2995,#2996,#2997,#2998));
#877=EDGE_LOOP('',(#2999));
#878=EDGE_LOOP('',(#3000));
#879=EDGE_LOOP('',(#3001,#3002,#3003,#3004));
#880=EDGE_LOOP('',(#3005));
#881=EDGE_LOOP('',(#3006));
#882=EDGE_LOOP('',(#3007,#3008,#3009,#3010));
#883=EDGE_LOOP('',(#3011));
#884=EDGE_LOOP('',(#3012,#3013,#3014,#3015));
#885=EDGE_LOOP('',(#3016,#3017,#3018,#3019));
#886=EDGE_LOOP('',(#3020,#3021,#3022,#3023));
#887=EDGE_LOOP('',(#3024));
#888=EDGE_LOOP('',(#3025));
#889=EDGE_LOOP('',(#3026,#3027,#3028,#3029));
#890=EDGE_LOOP('',(#3030,#3031,#3032,#3033));
#891=EDGE_LOOP('',(#3034,#3035,#3036,#3037));
#892=EDGE_LOOP('',(#3038));
#893=EDGE_LOOP('',(#3039,#3040,#3041,#3042));
#894=EDGE_LOOP('',(#3043,#3044,#3045,#3046));
#895=EDGE_LOOP('',(#3047,#3048,#3049,#3050));
#896=EDGE_LOOP('',(#3051,#3052,#3053,#3054));
#897=EDGE_LOOP('',(#3055,#3056,#3057,#3058));
#898=EDGE_LOOP('',(#3059,#3060,#3061,#3062));
#899=EDGE_LOOP('',(#3063,#3064,#3065,#3066,#3067,#3068));
#900=EDGE_LOOP('',(#3069,#3070,#3071,#3072,#3073,#3074));
#901=LINE('',#4947,#1135);
#902=LINE('',#4954,#1136);
#903=LINE('',#4961,#1137);
#904=LINE('',#4968,#1138);
#905=LINE('',#4996,#1139);
#906=LINE('',#5041,#1140);
#907=LINE('',#5086,#1141);
#908=LINE('',#5110,#1142);
#909=LINE('',#5117,#1143);
#910=LINE('',#5124,#1144);
#911=LINE('',#5131,#1145);
#912=LINE('',#5159,#1146);
#913=LINE('',#5204,#1147);
#914=LINE('',#5249,#1148);
#915=LINE('',#5273,#1149);
#916=LINE('',#5279,#1150);
#917=LINE('',#5285,#1151);
#918=LINE('',#5291,#1152);
#919=LINE('',#5297,#1153);
#920=LINE('',#5306,#1154);
#921=LINE('',#5315,#1155);
#922=LINE('',#5324,#1156);
#923=LINE('',#5333,#1157);
#924=LINE('',#5342,#1158);
#925=LINE('',#5348,#1159);
#926=LINE('',#5349,#1160);
#927=LINE('',#5350,#1161);
#928=LINE('',#5352,#1162);
#929=LINE('',#5353,#1163);
#930=LINE('',#5354,#1164);
#931=LINE('',#5356,#1165);
#932=LINE('',#5357,#1166);
#933=LINE('',#5358,#1167);
#934=LINE('',#5362,#1168);
#935=LINE('',#5364,#1169);
#936=LINE('',#5366,#1170);
#937=LINE('',#5367,#1171);
#938=LINE('',#5370,#1172);
#939=LINE('',#5372,#1173);
#940=LINE('',#5373,#1174);
#941=LINE('',#5376,#1175);
#942=LINE('',#5378,#1176);
#943=LINE('',#5379,#1177);
#944=LINE('',#5381,#1178);
#945=LINE('',#5382,#1179);
#946=LINE('',#5390,#1180);
#947=LINE('',#5396,#1181);
#948=LINE('',#5402,#1182);
#949=LINE('',#5408,#1183);
#950=LINE('',#5414,#1184);
#951=LINE('',#5420,#1185);
#952=LINE('',#5433,#1186);
#953=LINE('',#5437,#1187);
#954=LINE('',#5441,#1188);
#955=LINE('',#5447,#1189);
#956=LINE('',#5456,#1190);
#957=LINE('',#5462,#1191);
#958=LINE('',#5468,#1192);
#959=LINE('',#5474,#1193);
#960=LINE('',#5480,#1194);
#961=LINE('',#5486,#1195);
#962=LINE('',#5499,#1196);
#963=LINE('',#5503,#1197);
#964=LINE('',#5507,#1198);
#965=LINE('',#5513,#1199);
#966=LINE('',#5521,#1200);
#967=LINE('',#5523,#1201);
#968=LINE('',#5525,#1202);
#969=LINE('',#5527,#1203);
#970=LINE('',#5529,#1204);
#971=LINE('',#5530,#1205);
#972=LINE('',#5536,#1206);
#973=LINE('',#5538,#1207);
#974=LINE('',#5540,#1208);
#975=LINE('',#5542,#1209);
#976=LINE('',#5544,#1210);
#977=LINE('',#5545,#1211);
#978=LINE('',#5549,#1212);
#979=LINE('',#5550,#1213);
#980=LINE('',#5552,#1214);
#981=LINE('',#5554,#1215);
#982=LINE('',#5556,#1216);
#983=LINE('',#5558,#1217);
#984=LINE('',#5562,#1218);
#985=LINE('',#5570,#1219);
#986=LINE('',#5574,#1220);
#987=LINE('',#5578,#1221);
#988=LINE('',#5583,#1222);
#989=LINE('',#5588,#1223);
#990=LINE('',#5590,#1224);
#991=LINE('',#5592,#1225);
#992=LINE('',#5594,#1226);
#993=LINE('',#5596,#1227);
#994=LINE('',#5597,#1228);
#995=LINE('',#5602,#1229);
#996=LINE('',#5604,#1230);
#997=LINE('',#5605,#1231);
#998=LINE('',#5608,#1232);
#999=LINE('',#5609,#1233);
#1000=LINE('',#5612,#1234);
#1001=LINE('',#5613,#1235);
#1002=LINE('',#5616,#1236);
#1003=LINE('',#5617,#1237);
#1004=LINE('',#5620,#1238);
#1005=LINE('',#5621,#1239);
#1006=LINE('',#5623,#1240);
#1007=LINE('',#5627,#1241);
#1008=LINE('',#5634,#1242);
#1009=LINE('',#5636,#1243);
#1010=LINE('',#5638,#1244);
#1011=LINE('',#5639,#1245);
#1012=LINE('',#5642,#1246);
#1013=LINE('',#5644,#1247);
#1014=LINE('',#5645,#1248);
#1015=LINE('',#5648,#1249);
#1016=LINE('',#5650,#1250);
#1017=LINE('',#5651,#1251);
#1018=LINE('',#5653,#1252);
#1019=LINE('',#5654,#1253);
#1020=LINE('',#5661,#1254);
#1021=LINE('',#5670,#1255);
#1022=LINE('',#5679,#1256);
#1023=LINE('',#5688,#1257);
#1024=LINE('',#5697,#1258);
#1025=LINE('',#5705,#1259);
#1026=LINE('',#5709,#1260);
#1027=LINE('',#5713,#1261);
#1028=LINE('',#5717,#1262);
#1029=LINE('',#5722,#1263);
#1030=LINE('',#5731,#1264);
#1031=LINE('',#5736,#1265);
#1032=LINE('',#5741,#1266);
#1033=LINE('',#5746,#1267);
#1034=LINE('',#5748,#1268);
#1035=LINE('',#5750,#1269);
#1036=LINE('',#5751,#1270);
#1037=LINE('',#5754,#1271);
#1038=LINE('',#5756,#1272);
#1039=LINE('',#5757,#1273);
#1040=LINE('',#5760,#1274);
#1041=LINE('',#5762,#1275);
#1042=LINE('',#5763,#1276);
#1043=LINE('',#5765,#1277);
#1044=LINE('',#5766,#1278);
#1045=LINE('',#5774,#1279);
#1046=LINE('',#5780,#1280);
#1047=LINE('',#5786,#1281);
#1048=LINE('',#5792,#1282);
#1049=LINE('',#5798,#1283);
#1050=LINE('',#5804,#1284);
#1051=LINE('',#5810,#1285);
#1052=LINE('',#5815,#1286);
#1053=LINE('',#5817,#1287);
#1054=LINE('',#5819,#1288);
#1055=LINE('',#5820,#1289);
#1056=LINE('',#5823,#1290);
#1057=LINE('',#5825,#1291);
#1058=LINE('',#5826,#1292);
#1059=LINE('',#5829,#1293);
#1060=LINE('',#5831,#1294);
#1061=LINE('',#5832,#1295);
#1062=LINE('',#5834,#1296);
#1063=LINE('',#5835,#1297);
#1064=LINE('',#5843,#1298);
#1065=LINE('',#5851,#1299);
#1066=LINE('',#5853,#1300);
#1067=LINE('',#5855,#1301);
#1068=LINE('',#5857,#1302);
#1069=LINE('',#5859,#1303);
#1070=LINE('',#5860,#1304);
#1071=LINE('',#5865,#1305);
#1072=LINE('',#5867,#1306);
#1073=LINE('',#5868,#1307);
#1074=LINE('',#5871,#1308);
#1075=LINE('',#5872,#1309);
#1076=LINE('',#5875,#1310);
#1077=LINE('',#5876,#1311);
#1078=LINE('',#5879,#1312);
#1079=LINE('',#5880,#1313);
#1080=LINE('',#5883,#1314);
#1081=LINE('',#5884,#1315);
#1082=LINE('',#5886,#1316);
#1083=LINE('',#5890,#1317);
#1084=LINE('',#5894,#1318);
#1085=LINE('',#5903,#1319);
#1086=LINE('',#5911,#1320);
#1087=LINE('',#5913,#1321);
#1088=LINE('',#5915,#1322);
#1089=LINE('',#5917,#1323);
#1090=LINE('',#5919,#1324);
#1091=LINE('',#5920,#1325);
#1092=LINE('',#5926,#1326);
#1093=LINE('',#5928,#1327);
#1094=LINE('',#5930,#1328);
#1095=LINE('',#5932,#1329);
#1096=LINE('',#5934,#1330);
#1097=LINE('',#5935,#1331);
#1098=LINE('',#5939,#1332);
#1099=LINE('',#5940,#1333);
#1100=LINE('',#5942,#1334);
#1101=LINE('',#5944,#1335);
#1102=LINE('',#5946,#1336);
#1103=LINE('',#5948,#1337);
#1104=LINE('',#5955,#1338);
#1105=LINE('',#5961,#1339);
#1106=LINE('',#5965,#1340);
#1107=LINE('',#5970,#1341);
#1108=LINE('',#5980,#1342);
#1109=LINE('',#5987,#1343);
#1110=LINE('',#5992,#1344);
#1111=LINE('',#6002,#1345);
#1112=LINE('',#6006,#1346);
#1113=LINE('',#6010,#1347);
#1114=LINE('',#6017,#1348);
#1115=LINE('',#6021,#1349);
#1116=LINE('',#6025,#1350);
#1117=LINE('',#6030,#1351);
#1118=LINE('',#6032,#1352);
#1119=LINE('',#6034,#1353);
#1120=LINE('',#6035,#1354);
#1121=LINE('',#6038,#1355);
#1122=LINE('',#6040,#1356);
#1123=LINE('',#6041,#1357);
#1124=LINE('',#6044,#1358);
#1125=LINE('',#6046,#1359);
#1126=LINE('',#6047,#1360);
#1127=LINE('',#6050,#1361);
#1128=LINE('',#6052,#1362);
#1129=LINE('',#6053,#1363);
#1130=LINE('',#6056,#1364);
#1131=LINE('',#6058,#1365);
#1132=LINE('',#6059,#1366);
#1133=LINE('',#6061,#1367);
#1134=LINE('',#6062,#1368);
#1135=VECTOR('',#3913,0.165);
#1136=VECTOR('',#3922,0.165);
#1137=VECTOR('',#3931,0.165);
#1138=VECTOR('',#3940,0.165);
#1139=VECTOR('',#3947,0.2);
#1140=VECTOR('',#3952,0.2);
#1141=VECTOR('',#3957,0.2);
#1142=VECTOR('',#3964,0.165);
#1143=VECTOR('',#3973,0.165);
#1144=VECTOR('',#3982,0.165);
#1145=VECTOR('',#3991,0.165);
#1146=VECTOR('',#3998,0.2);
#1147=VECTOR('',#4003,0.2);
#1148=VECTOR('',#4008,0.2);
#1149=VECTOR('',#4015,0.33);
#1150=VECTOR('',#4022,0.33);
#1151=VECTOR('',#4029,0.33);
#1152=VECTOR('',#4036,0.33);
#1153=VECTOR('',#4043,0.685);
#1154=VECTOR('',#4054,0.685);
#1155=VECTOR('',#4065,0.685);
#1156=VECTOR('',#4076,0.685);
#1157=VECTOR('',#4087,0.685);
#1158=VECTOR('',#4098,0.685);
#1159=VECTOR('',#4107,0.3);
#1160=VECTOR('',#4108,0.3);
#1161=VECTOR('',#4109,0.3);
#1162=VECTOR('',#4112,0.3);
#1163=VECTOR('',#4113,0.3);
#1164=VECTOR('',#4114,0.3);
#1165=VECTOR('',#4117,0.3);
#1166=VECTOR('',#4118,0.3);
#1167=VECTOR('',#4119,0.3);
#1168=VECTOR('',#4122,1.);
#1169=VECTOR('',#4123,1.);
#1170=VECTOR('',#4124,1.);
#1171=VECTOR('',#4125,1.);
#1172=VECTOR('',#4128,1.);
#1173=VECTOR('',#4129,1.);
#1174=VECTOR('',#4130,1.);
#1175=VECTOR('',#4133,1.);
#1176=VECTOR('',#4134,1.);
#1177=VECTOR('',#4135,1.);
#1178=VECTOR('',#4138,1.);
#1179=VECTOR('',#4139,1.);
#1180=VECTOR('',#4150,0.05);
#1181=VECTOR('',#4157,0.05);
#1182=VECTOR('',#4164,0.05);
#1183=VECTOR('',#4171,0.05);
#1184=VECTOR('',#4178,0.05);
#1185=VECTOR('',#4185,0.05);
#1186=VECTOR('',#4202,0.9);
#1187=VECTOR('',#4207,0.45);
#1188=VECTOR('',#4212,0.3);
#1189=VECTOR('',#4219,0.685);
#1190=VECTOR('',#4232,0.05);
#1191=VECTOR('',#4239,0.05);
#1192=VECTOR('',#4246,0.05);
#1193=VECTOR('',#4253,0.05);
#1194=VECTOR('',#4260,0.05);
#1195=VECTOR('',#4267,0.05);
#1196=VECTOR('',#4284,0.9);
#1197=VECTOR('',#4289,0.45);
#1198=VECTOR('',#4294,0.3);
#1199=VECTOR('',#4301,0.685);
#1200=VECTOR('',#4312,1.);
#1201=VECTOR('',#4313,1.);
#1202=VECTOR('',#4314,1.);
#1203=VECTOR('',#4315,1.);
#1204=VECTOR('',#4316,1.);
#1205=VECTOR('',#4317,1.);
#1206=VECTOR('',#4322,1.);
#1207=VECTOR('',#4323,1.);
#1208=VECTOR('',#4324,1.);
#1209=VECTOR('',#4325,1.);
#1210=VECTOR('',#4326,1.);
#1211=VECTOR('',#4327,1.);
#1212=VECTOR('',#4332,1.);
#1213=VECTOR('',#4333,1.);
#1214=VECTOR('',#4336,1.);
#1215=VECTOR('',#4339,1.);
#1216=VECTOR('',#4342,1.);
#1217=VECTOR('',#4345,1.);
#1218=VECTOR('',#4350,0.685);
#1219=VECTOR('',#4361,0.645);
#1220=VECTOR('',#4366,0.685);
#1221=VECTOR('',#4371,0.645);
#1222=VECTOR('',#4378,0.46);
#1223=VECTOR('',#4383,1.);
#1224=VECTOR('',#4384,1.);
#1225=VECTOR('',#4385,1.);
#1226=VECTOR('',#4386,1.);
#1227=VECTOR('',#4387,1.);
#1228=VECTOR('',#4388,1.);
#1229=VECTOR('',#4393,1.);
#1230=VECTOR('',#4394,1.);
#1231=VECTOR('',#4395,1.);
#1232=VECTOR('',#4398,1.);
#1233=VECTOR('',#4399,1.);
#1234=VECTOR('',#4402,1.);
#1235=VECTOR('',#4403,1.);
#1236=VECTOR('',#4406,1.);
#1237=VECTOR('',#4407,1.);
#1238=VECTOR('',#4410,1.);
#1239=VECTOR('',#4411,1.);
#1240=VECTOR('',#4414,1.);
#1241=VECTOR('',#4419,0.685);
#1242=VECTOR('',#4428,1.);
#1243=VECTOR('',#4429,1.);
#1244=VECTOR('',#4430,1.);
#1245=VECTOR('',#4431,1.);
#1246=VECTOR('',#4434,1.);
#1247=VECTOR('',#4435,1.);
#1248=VECTOR('',#4436,1.);
#1249=VECTOR('',#4439,1.);
#1250=VECTOR('',#4440,1.);
#1251=VECTOR('',#4441,1.);
#1252=VECTOR('',#4444,1.);
#1253=VECTOR('',#4445,1.);
#1254=VECTOR('',#4454,0.685);
#1255=VECTOR('',#4467,0.4);
#1256=VECTOR('',#4478,0.4);
#1257=VECTOR('',#4489,0.4);
#1258=VECTOR('',#4500,0.4);
#1259=VECTOR('',#4511,0.225);
#1260=VECTOR('',#4516,0.225);
#1261=VECTOR('',#4521,0.225);
#1262=VECTOR('',#4526,0.225);
#1263=VECTOR('',#4531,0.685);
#1264=VECTOR('',#4542,0.2);
#1265=VECTOR('',#4549,0.2);
#1266=VECTOR('',#4554,0.2);
#1267=VECTOR('',#4559,1.);
#1268=VECTOR('',#4560,1.);
#1269=VECTOR('',#4561,1.);
#1270=VECTOR('',#4562,1.);
#1271=VECTOR('',#4565,1.);
#1272=VECTOR('',#4566,1.);
#1273=VECTOR('',#4567,1.);
#1274=VECTOR('',#4570,1.);
#1275=VECTOR('',#4571,1.);
#1276=VECTOR('',#4572,1.);
#1277=VECTOR('',#4575,1.);
#1278=VECTOR('',#4576,1.);
#1279=VECTOR('',#4587,0.225);
#1280=VECTOR('',#4594,0.225);
#1281=VECTOR('',#4601,0.225);
#1282=VECTOR('',#4608,0.225);
#1283=VECTOR('',#4615,0.2);
#1284=VECTOR('',#4622,0.2);
#1285=VECTOR('',#4629,0.2);
#1286=VECTOR('',#4634,1.);
#1287=VECTOR('',#4635,1.);
#1288=VECTOR('',#4636,1.);
#1289=VECTOR('',#4637,1.);
#1290=VECTOR('',#4640,1.);
#1291=VECTOR('',#4641,1.);
#1292=VECTOR('',#4642,1.);
#1293=VECTOR('',#4645,1.);
#1294=VECTOR('',#4646,1.);
#1295=VECTOR('',#4647,1.);
#1296=VECTOR('',#4650,1.);
#1297=VECTOR('',#4651,1.);
#1298=VECTOR('',#4662,0.515);
#1299=VECTOR('',#4671,1.);
#1300=VECTOR('',#4672,1.);
#1301=VECTOR('',#4673,1.);
#1302=VECTOR('',#4674,1.);
#1303=VECTOR('',#4675,1.);
#1304=VECTOR('',#4676,1.);
#1305=VECTOR('',#4681,1.);
#1306=VECTOR('',#4682,1.);
#1307=VECTOR('',#4683,1.);
#1308=VECTOR('',#4686,1.);
#1309=VECTOR('',#4687,1.);
#1310=VECTOR('',#4690,1.);
#1311=VECTOR('',#4691,1.);
#1312=VECTOR('',#4694,1.);
#1313=VECTOR('',#4695,1.);
#1314=VECTOR('',#4698,1.);
#1315=VECTOR('',#4699,1.);
#1316=VECTOR('',#4702,1.);
#1317=VECTOR('',#4707,0.2);
#1318=VECTOR('',#4712,0.685);
#1319=VECTOR('',#4725,0.43);
#1320=VECTOR('',#4734,1.);
#1321=VECTOR('',#4735,1.);
#1322=VECTOR('',#4736,1.);
#1323=VECTOR('',#4737,1.);
#1324=VECTOR('',#4738,1.);
#1325=VECTOR('',#4739,1.);
#1326=VECTOR('',#4744,1.);
#1327=VECTOR('',#4745,1.);
#1328=VECTOR('',#4746,1.);
#1329=VECTOR('',#4747,1.);
#1330=VECTOR('',#4748,1.);
#1331=VECTOR('',#4749,1.);
#1332=VECTOR('',#4754,1.);
#1333=VECTOR('',#4755,1.);
#1334=VECTOR('',#4758,1.);
#1335=VECTOR('',#4761,1.);
#1336=VECTOR('',#4764,1.);
#1337=VECTOR('',#4767,1.);
#1338=VECTOR('',#4776,0.46);
#1339=VECTOR('',#4785,0.525);
#1340=VECTOR('',#4790,0.515);
#1341=VECTOR('',#4797,0.2);
#1342=VECTOR('',#4810,0.475);
#1343=VECTOR('',#4819,0.355);
#1344=VECTOR('',#4826,0.31);
#1345=VECTOR('',#4841,0.325);
#1346=VECTOR('',#4846,0.35);
#1347=VECTOR('',#4851,0.335);
#1348=VECTOR('',#4860,0.21);
#1349=VECTOR('',#4865,0.2);
#1350=VECTOR('',#4870,0.18);
#1351=VECTOR('',#4875,1.);
#1352=VECTOR('',#4876,1.);
#1353=VECTOR('',#4877,1.);
#1354=VECTOR('',#4878,1.);
#1355=VECTOR('',#4881,1.);
#1356=VECTOR('',#4882,1.);
#1357=VECTOR('',#4883,1.);
#1358=VECTOR('',#4886,1.);
#1359=VECTOR('',#4887,1.);
#1360=VECTOR('',#4888,1.);
#1361=VECTOR('',#4891,1.);
#1362=VECTOR('',#4892,1.);
#1363=VECTOR('',#4893,1.);
#1364=VECTOR('',#4896,1.);
#1365=VECTOR('',#4897,1.);
#1366=VECTOR('',#4898,1.);
#1367=VECTOR('',#4901,1.);
#1368=VECTOR('',#4902,1.);
#1369=CIRCLE('',#3507,0.165);
#1370=CIRCLE('',#3508,0.165);
#1371=CIRCLE('',#3511,0.165);
#1372=CIRCLE('',#3512,0.165);
#1373=CIRCLE('',#3515,0.165);
#1374=CIRCLE('',#3516,0.165);
#1375=CIRCLE('',#3519,0.165);
#1376=CIRCLE('',#3520,0.165);
#1377=CIRCLE('',#3523,0.2);
#1378=CIRCLE('',#3525,0.2);
#1379=CIRCLE('',#3527,0.2);
#1380=CIRCLE('',#3529,0.165);
#1381=CIRCLE('',#3530,0.165);
#1382=CIRCLE('',#3533,0.165);
#1383=CIRCLE('',#3534,0.165);
#1384=CIRCLE('',#3537,0.165);
#1385=CIRCLE('',#3538,0.165);
#1386=CIRCLE('',#3541,0.165);
#1387=CIRCLE('',#3542,0.165);
#1388=CIRCLE('',#3545,0.2);
#1389=CIRCLE('',#3547,0.2);
#1390=CIRCLE('',#3549,0.2);
#1391=CIRCLE('',#3551,0.33);
#1392=CIRCLE('',#3552,0.33);
#1393=CIRCLE('',#3554,0.33);
#1394=CIRCLE('',#3555,0.33);
#1395=CIRCLE('',#3557,0.33);
#1396=CIRCLE('',#3558,0.33);
#1397=CIRCLE('',#3560,0.33);
#1398=CIRCLE('',#3561,0.33);
#1399=CIRCLE('',#3563,0.685);
#1400=CIRCLE('',#3564,0.685);
#1401=CIRCLE('',#3566,0.3);
#1402=CIRCLE('',#3568,0.685);
#1403=CIRCLE('',#3569,0.685);
#1404=CIRCLE('',#3571,0.3);
#1405=CIRCLE('',#3573,0.685);
#1406=CIRCLE('',#3574,0.685);
#1407=CIRCLE('',#3576,0.3);
#1408=CIRCLE('',#3578,0.685);
#1409=CIRCLE('',#3579,0.685);
#1410=CIRCLE('',#3581,0.3);
#1411=CIRCLE('',#3583,0.685);
#1412=CIRCLE('',#3584,0.685);
#1413=CIRCLE('',#3586,0.3);
#1414=CIRCLE('',#3588,0.685);
#1415=CIRCLE('',#3589,0.685);
#1416=CIRCLE('',#3591,0.3);
#1417=CIRCLE('',#3603,0.05);
#1418=CIRCLE('',#3604,0.05);
#1419=CIRCLE('',#3606,0.05);
#1420=CIRCLE('',#3607,0.05);
#1421=CIRCLE('',#3609,0.05);
#1422=CIRCLE('',#3610,0.05);
#1423=CIRCLE('',#3612,0.05);
#1424=CIRCLE('',#3613,0.05);
#1425=CIRCLE('',#3615,0.05);
#1426=CIRCLE('',#3616,0.05);
#1427=CIRCLE('',#3618,0.05);
#1428=CIRCLE('',#3619,0.05);
#1429=CIRCLE('',#3621,0.3);
#1430=CIRCLE('',#3623,0.9);
#1431=CIRCLE('',#3624,0.45);
#1432=CIRCLE('',#3626,0.9);
#1433=CIRCLE('',#3629,0.45);
#1434=CIRCLE('',#3631,0.3);
#1435=CIRCLE('',#3633,0.685);
#1436=CIRCLE('',#3634,0.685);
#1437=CIRCLE('',#3639,0.05);
#1438=CIRCLE('',#3640,0.05);
#1439=CIRCLE('',#3642,0.05);
#1440=CIRCLE('',#3643,0.05);
#1441=CIRCLE('',#3645,0.05);
#1442=CIRCLE('',#3646,0.05);
#1443=CIRCLE('',#3648,0.05);
#1444=CIRCLE('',#3649,0.05);
#1445=CIRCLE('',#3651,0.05);
#1446=CIRCLE('',#3652,0.05);
#1447=CIRCLE('',#3654,0.05);
#1448=CIRCLE('',#3655,0.05);
#1449=CIRCLE('',#3657,0.3);
#1450=CIRCLE('',#3659,0.9);
#1451=CIRCLE('',#3660,0.45);
#1452=CIRCLE('',#3662,0.9);
#1453=CIRCLE('',#3665,0.45);
#1454=CIRCLE('',#3667,0.3);
#1455=CIRCLE('',#3669,0.685);
#1456=CIRCLE('',#3670,0.685);
#1457=CIRCLE('',#3675,0.685);
#1458=CIRCLE('',#3677,0.685);
#1459=CIRCLE('',#3685,0.685);
#1460=CIRCLE('',#3687,0.605);
#1461=CIRCLE('',#3688,0.46);
#1462=CIRCLE('',#3691,0.685);
#1463=CIRCLE('',#3693,0.605);
#1464=CIRCLE('',#3695,0.46);
#1465=CIRCLE('',#3699,0.685);
#1466=CIRCLE('',#3708,0.685);
#1467=CIRCLE('',#3717,0.685);
#1468=CIRCLE('',#3719,0.685);
#1469=CIRCLE('',#3724,0.4);
#1470=CIRCLE('',#3725,0.4);
#1471=CIRCLE('',#3727,0.225);
#1472=CIRCLE('',#3729,0.4);
#1473=CIRCLE('',#3730,0.4);
#1474=CIRCLE('',#3732,0.225);
#1475=CIRCLE('',#3734,0.4);
#1476=CIRCLE('',#3735,0.4);
#1477=CIRCLE('',#3737,0.225);
#1478=CIRCLE('',#3739,0.4);
#1479=CIRCLE('',#3740,0.4);
#1480=CIRCLE('',#3742,0.225);
#1481=CIRCLE('',#3744,0.225);
#1482=CIRCLE('',#3746,0.225);
#1483=CIRCLE('',#3748,0.225);
#1484=CIRCLE('',#3750,0.225);
#1485=CIRCLE('',#3752,0.685);
#1486=CIRCLE('',#3753,0.685);
#1487=CIRCLE('',#3755,0.2);
#1488=CIRCLE('',#3757,0.2);
#1489=CIRCLE('',#3758,0.2);
#1490=CIRCLE('',#3760,0.2);
#1491=CIRCLE('',#3762,0.2);
#1492=CIRCLE('',#3763,0.2);
#1493=CIRCLE('',#3772,0.225);
#1494=CIRCLE('',#3773,0.225);
#1495=CIRCLE('',#3775,0.225);
#1496=CIRCLE('',#3776,0.225);
#1497=CIRCLE('',#3778,0.225);
#1498=CIRCLE('',#3779,0.225);
#1499=CIRCLE('',#3781,0.225);
#1500=CIRCLE('',#3782,0.225);
#1501=CIRCLE('',#3784,0.2);
#1502=CIRCLE('',#3785,0.2);
#1503=CIRCLE('',#3787,0.2);
#1504=CIRCLE('',#3788,0.2);
#1505=CIRCLE('',#3790,0.2);
#1506=CIRCLE('',#3791,0.2);
#1507=CIRCLE('',#3800,0.515);
#1508=CIRCLE('',#3801,0.515);
#1509=CIRCLE('',#3803,0.2);
#1510=CIRCLE('',#3805,0.685);
#1511=CIRCLE('',#3814,0.2);
#1512=CIRCLE('',#3816,0.685);
#1513=CIRCLE('',#3821,0.43);
#1514=CIRCLE('',#3822,0.43);
#1515=CIRCLE('',#3824,0.2);
#1516=CIRCLE('',#3826,0.525);
#1517=CIRCLE('',#3828,0.515);
#1518=CIRCLE('',#3836,0.46);
#1519=CIRCLE('',#3838,0.46);
#1520=CIRCLE('',#3840,0.525);
#1521=CIRCLE('',#3843,0.515);
#1522=CIRCLE('',#3845,0.2);
#1523=CIRCLE('',#3849,0.475);
#1524=CIRCLE('',#3850,0.31);
#1525=CIRCLE('',#3852,0.475);
#1526=CIRCLE('',#3854,0.355);
#1527=CIRCLE('',#3856,0.355);
#1528=CIRCLE('',#3858,0.31);
#1529=CIRCLE('',#3864,0.3);
#1530=CIRCLE('',#3866,0.35);
#1531=CIRCLE('',#3868,0.35);
#1532=CIRCLE('',#3870,0.32);
#1533=CIRCLE('',#3872,0.22);
#1534=CIRCLE('',#3874,0.1954);
#1535=CIRCLE('',#3876,0.1954);
#1536=CIRCLE('',#3878,0.16);
#1537=VERTEX_POINT('',#4944);
#1538=VERTEX_POINT('',#4946);
#1539=VERTEX_POINT('',#4951);
#1540=VERTEX_POINT('',#4953);
#1541=VERTEX_POINT('',#4958);
#1542=VERTEX_POINT('',#4960);
#1543=VERTEX_POINT('',#4965);
#1544=VERTEX_POINT('',#4967);
#1545=VERTEX_POINT('',#4972);
#1546=VERTEX_POINT('',#4973);
#1547=VERTEX_POINT('',#4984);
#1548=VERTEX_POINT('',#4995);
#1549=VERTEX_POINT('',#5017);
#1550=VERTEX_POINT('',#5018);
#1551=VERTEX_POINT('',#5029);
#1552=VERTEX_POINT('',#5040);
#1553=VERTEX_POINT('',#5062);
#1554=VERTEX_POINT('',#5063);
#1555=VERTEX_POINT('',#5074);
#1556=VERTEX_POINT('',#5085);
#1557=VERTEX_POINT('',#5107);
#1558=VERTEX_POINT('',#5109);
#1559=VERTEX_POINT('',#5114);
#1560=VERTEX_POINT('',#5116);
#1561=VERTEX_POINT('',#5121);
#1562=VERTEX_POINT('',#5123);
#1563=VERTEX_POINT('',#5128);
#1564=VERTEX_POINT('',#5130);
#1565=VERTEX_POINT('',#5135);
#1566=VERTEX_POINT('',#5136);
#1567=VERTEX_POINT('',#5147);
#1568=VERTEX_POINT('',#5158);
#1569=VERTEX_POINT('',#5180);
#1570=VERTEX_POINT('',#5181);
#1571=VERTEX_POINT('',#5192);
#1572=VERTEX_POINT('',#5203);
#1573=VERTEX_POINT('',#5225);
#1574=VERTEX_POINT('',#5226);
#1575=VERTEX_POINT('',#5237);
#1576=VERTEX_POINT('',#5248);
#1577=VERTEX_POINT('',#5270);
#1578=VERTEX_POINT('',#5272);
#1579=VERTEX_POINT('',#5276);
#1580=VERTEX_POINT('',#5278);
#1581=VERTEX_POINT('',#5282);
#1582=VERTEX_POINT('',#5284);
#1583=VERTEX_POINT('',#5288);
#1584=VERTEX_POINT('',#5290);
#1585=VERTEX_POINT('',#5294);
#1586=VERTEX_POINT('',#5296);
#1587=VERTEX_POINT('',#5300);
#1588=VERTEX_POINT('',#5303);
#1589=VERTEX_POINT('',#5305);
#1590=VERTEX_POINT('',#5309);
#1591=VERTEX_POINT('',#5312);
#1592=VERTEX_POINT('',#5314);
#1593=VERTEX_POINT('',#5318);
#1594=VERTEX_POINT('',#5321);
#1595=VERTEX_POINT('',#5323);
#1596=VERTEX_POINT('',#5327);
#1597=VERTEX_POINT('',#5330);
#1598=VERTEX_POINT('',#5332);
#1599=VERTEX_POINT('',#5336);
#1600=VERTEX_POINT('',#5339);
#1601=VERTEX_POINT('',#5341);
#1602=VERTEX_POINT('',#5345);
#1603=VERTEX_POINT('',#5360);
#1604=VERTEX_POINT('',#5361);
#1605=VERTEX_POINT('',#5363);
#1606=VERTEX_POINT('',#5365);
#1607=VERTEX_POINT('',#5369);
#1608=VERTEX_POINT('',#5371);
#1609=VERTEX_POINT('',#5375);
#1610=VERTEX_POINT('',#5377);
#1611=VERTEX_POINT('',#5387);
#1612=VERTEX_POINT('',#5389);
#1613=VERTEX_POINT('',#5393);
#1614=VERTEX_POINT('',#5395);
#1615=VERTEX_POINT('',#5399);
#1616=VERTEX_POINT('',#5401);
#1617=VERTEX_POINT('',#5405);
#1618=VERTEX_POINT('',#5407);
#1619=VERTEX_POINT('',#5411);
#1620=VERTEX_POINT('',#5413);
#1621=VERTEX_POINT('',#5417);
#1622=VERTEX_POINT('',#5419);
#1623=VERTEX_POINT('',#5423);
#1624=VERTEX_POINT('',#5426);
#1625=VERTEX_POINT('',#5428);
#1626=VERTEX_POINT('',#5431);
#1627=VERTEX_POINT('',#5436);
#1628=VERTEX_POINT('',#5440);
#1629=VERTEX_POINT('',#5444);
#1630=VERTEX_POINT('',#5446);
#1631=VERTEX_POINT('',#5453);
#1632=VERTEX_POINT('',#5455);
#1633=VERTEX_POINT('',#5459);
#1634=VERTEX_POINT('',#5461);
#1635=VERTEX_POINT('',#5465);
#1636=VERTEX_POINT('',#5467);
#1637=VERTEX_POINT('',#5471);
#1638=VERTEX_POINT('',#5473);
#1639=VERTEX_POINT('',#5477);
#1640=VERTEX_POINT('',#5479);
#1641=VERTEX_POINT('',#5483);
#1642=VERTEX_POINT('',#5485);
#1643=VERTEX_POINT('',#5489);
#1644=VERTEX_POINT('',#5492);
#1645=VERTEX_POINT('',#5494);
#1646=VERTEX_POINT('',#5497);
#1647=VERTEX_POINT('',#5502);
#1648=VERTEX_POINT('',#5506);
#1649=VERTEX_POINT('',#5510);
#1650=VERTEX_POINT('',#5512);
#1651=VERTEX_POINT('',#5519);
#1652=VERTEX_POINT('',#5520);
#1653=VERTEX_POINT('',#5522);
#1654=VERTEX_POINT('',#5524);
#1655=VERTEX_POINT('',#5526);
#1656=VERTEX_POINT('',#5528);
#1657=VERTEX_POINT('',#5531);
#1658=VERTEX_POINT('',#5534);
#1659=VERTEX_POINT('',#5535);
#1660=VERTEX_POINT('',#5537);
#1661=VERTEX_POINT('',#5539);
#1662=VERTEX_POINT('',#5541);
#1663=VERTEX_POINT('',#5543);
#1664=VERTEX_POINT('',#5546);
#1665=VERTEX_POINT('',#5561);
#1666=VERTEX_POINT('',#5565);
#1667=VERTEX_POINT('',#5567);
#1668=VERTEX_POINT('',#5572);
#1669=VERTEX_POINT('',#5576);
#1670=VERTEX_POINT('',#5580);
#1671=VERTEX_POINT('',#5586);
#1672=VERTEX_POINT('',#5587);
#1673=VERTEX_POINT('',#5589);
#1674=VERTEX_POINT('',#5591);
#1675=VERTEX_POINT('',#5593);
#1676=VERTEX_POINT('',#5595);
#1677=VERTEX_POINT('',#5598);
#1678=VERTEX_POINT('',#5601);
#1679=VERTEX_POINT('',#5603);
#1680=VERTEX_POINT('',#5607);
#1681=VERTEX_POINT('',#5611);
#1682=VERTEX_POINT('',#5615);
#1683=VERTEX_POINT('',#5619);
#1684=VERTEX_POINT('',#5626);
#1685=VERTEX_POINT('',#5632);
#1686=VERTEX_POINT('',#5633);
#1687=VERTEX_POINT('',#5635);
#1688=VERTEX_POINT('',#5637);
#1689=VERTEX_POINT('',#5641);
#1690=VERTEX_POINT('',#5643);
#1691=VERTEX_POINT('',#5647);
#1692=VERTEX_POINT('',#5649);
#1693=VERTEX_POINT('',#5657);
#1694=VERTEX_POINT('',#5660);
#1695=VERTEX_POINT('',#5667);
#1696=VERTEX_POINT('',#5669);
#1697=VERTEX_POINT('',#5673);
#1698=VERTEX_POINT('',#5676);
#1699=VERTEX_POINT('',#5678);
#1700=VERTEX_POINT('',#5682);
#1701=VERTEX_POINT('',#5685);
#1702=VERTEX_POINT('',#5687);
#1703=VERTEX_POINT('',#5691);
#1704=VERTEX_POINT('',#5694);
#1705=VERTEX_POINT('',#5696);
#1706=VERTEX_POINT('',#5700);
#1707=VERTEX_POINT('',#5703);
#1708=VERTEX_POINT('',#5707);
#1709=VERTEX_POINT('',#5711);
#1710=VERTEX_POINT('',#5715);
#1711=VERTEX_POINT('',#5719);
#1712=VERTEX_POINT('',#5721);
#1713=VERTEX_POINT('',#5725);
#1714=VERTEX_POINT('',#5728);
#1715=VERTEX_POINT('',#5730);
#1716=VERTEX_POINT('',#5734);
#1717=VERTEX_POINT('',#5738);
#1718=VERTEX_POINT('',#5740);
#1719=VERTEX_POINT('',#5744);
#1720=VERTEX_POINT('',#5745);
#1721=VERTEX_POINT('',#5747);
#1722=VERTEX_POINT('',#5749);
#1723=VERTEX_POINT('',#5753);
#1724=VERTEX_POINT('',#5755);
#1725=VERTEX_POINT('',#5759);
#1726=VERTEX_POINT('',#5761);
#1727=VERTEX_POINT('',#5771);
#1728=VERTEX_POINT('',#5773);
#1729=VERTEX_POINT('',#5777);
#1730=VERTEX_POINT('',#5779);
#1731=VERTEX_POINT('',#5783);
#1732=VERTEX_POINT('',#5785);
#1733=VERTEX_POINT('',#5789);
#1734=VERTEX_POINT('',#5791);
#1735=VERTEX_POINT('',#5795);
#1736=VERTEX_POINT('',#5797);
#1737=VERTEX_POINT('',#5801);
#1738=VERTEX_POINT('',#5803);
#1739=VERTEX_POINT('',#5807);
#1740=VERTEX_POINT('',#5809);
#1741=VERTEX_POINT('',#5813);
#1742=VERTEX_POINT('',#5814);
#1743=VERTEX_POINT('',#5816);
#1744=VERTEX_POINT('',#5818);
#1745=VERTEX_POINT('',#5822);
#1746=VERTEX_POINT('',#5824);
#1747=VERTEX_POINT('',#5828);
#1748=VERTEX_POINT('',#5830);
#1749=VERTEX_POINT('',#5840);
#1750=VERTEX_POINT('',#5842);
#1751=VERTEX_POINT('',#5846);
#1752=VERTEX_POINT('',#5849);
#1753=VERTEX_POINT('',#5850);
#1754=VERTEX_POINT('',#5852);
#1755=VERTEX_POINT('',#5854);
#1756=VERTEX_POINT('',#5856);
#1757=VERTEX_POINT('',#5858);
#1758=VERTEX_POINT('',#5861);
#1759=VERTEX_POINT('',#5864);
#1760=VERTEX_POINT('',#5866);
#1761=VERTEX_POINT('',#5870);
#1762=VERTEX_POINT('',#5874);
#1763=VERTEX_POINT('',#5878);
#1764=VERTEX_POINT('',#5882);
#1765=VERTEX_POINT('',#5889);
#1766=VERTEX_POINT('',#5893);
#1767=VERTEX_POINT('',#5900);
#1768=VERTEX_POINT('',#5902);
#1769=VERTEX_POINT('',#5906);
#1770=VERTEX_POINT('',#5909);
#1771=VERTEX_POINT('',#5910);
#1772=VERTEX_POINT('',#5912);
#1773=VERTEX_POINT('',#5914);
#1774=VERTEX_POINT('',#5916);
#1775=VERTEX_POINT('',#5918);
#1776=VERTEX_POINT('',#5921);
#1777=VERTEX_POINT('',#5924);
#1778=VERTEX_POINT('',#5925);
#1779=VERTEX_POINT('',#5927);
#1780=VERTEX_POINT('',#5929);
#1781=VERTEX_POINT('',#5931);
#1782=VERTEX_POINT('',#5933);
#1783=VERTEX_POINT('',#5936);
#1784=VERTEX_POINT('',#5951);
#1785=VERTEX_POINT('',#5954);
#1786=VERTEX_POINT('',#5958);
#1787=VERTEX_POINT('',#5963);
#1788=VERTEX_POINT('',#5967);
#1789=VERTEX_POINT('',#5973);
#1790=VERTEX_POINT('',#5975);
#1791=VERTEX_POINT('',#5978);
#1792=VERTEX_POINT('',#5982);
#1793=VERTEX_POINT('',#5985);
#1794=VERTEX_POINT('',#5989);
#1795=VERTEX_POINT('',#5997);
#1796=VERTEX_POINT('',#6000);
#1797=VERTEX_POINT('',#6004);
#1798=VERTEX_POINT('',#6008);
#1799=VERTEX_POINT('',#6012);
#1800=VERTEX_POINT('',#6015);
#1801=VERTEX_POINT('',#6019);
#1802=VERTEX_POINT('',#6023);
#1803=VERTEX_POINT('',#6028);
#1804=VERTEX_POINT('',#6029);
#1805=VERTEX_POINT('',#6031);
#1806=VERTEX_POINT('',#6033);
#1807=VERTEX_POINT('',#6037);
#1808=VERTEX_POINT('',#6039);
#1809=VERTEX_POINT('',#6043);
#1810=VERTEX_POINT('',#6045);
#1811=VERTEX_POINT('',#6049);
#1812=VERTEX_POINT('',#6051);
#1813=VERTEX_POINT('',#6055);
#1814=VERTEX_POINT('',#6057);
#1815=EDGE_CURVE('',#1537,#1537,#1369,.T.);
#1816=EDGE_CURVE('',#1537,#1538,#901,.T.);
#1817=EDGE_CURVE('',#1538,#1538,#1370,.T.);
#1818=EDGE_CURVE('',#1539,#1539,#1371,.T.);
#1819=EDGE_CURVE('',#1539,#1540,#902,.T.);
#1820=EDGE_CURVE('',#1540,#1540,#1372,.T.);
#1821=EDGE_CURVE('',#1541,#1541,#1373,.T.);
#1822=EDGE_CURVE('',#1541,#1542,#903,.T.);
#1823=EDGE_CURVE('',#1542,#1542,#1374,.T.);
#1824=EDGE_CURVE('',#1543,#1543,#1375,.T.);
#1825=EDGE_CURVE('',#1543,#1544,#904,.T.);
#1826=EDGE_CURVE('',#1544,#1544,#1376,.T.);
#1827=EDGE_CURVE('',#1545,#1546,#259,.T.);
#1828=EDGE_CURVE('',#1547,#1545,#260,.T.);
#1829=EDGE_CURVE('',#1547,#1548,#905,.T.);
#1830=EDGE_CURVE('',#1548,#1548,#1377,.T.);
#1831=EDGE_CURVE('',#1546,#1547,#261,.T.);
#1832=EDGE_CURVE('',#1549,#1550,#262,.T.);
#1833=EDGE_CURVE('',#1551,#1549,#263,.T.);
#1834=EDGE_CURVE('',#1551,#1552,#906,.T.);
#1835=EDGE_CURVE('',#1552,#1552,#1378,.T.);
#1836=EDGE_CURVE('',#1550,#1551,#264,.T.);
#1837=EDGE_CURVE('',#1553,#1554,#265,.T.);
#1838=EDGE_CURVE('',#1555,#1553,#266,.T.);
#1839=EDGE_CURVE('',#1555,#1556,#907,.T.);
#1840=EDGE_CURVE('',#1556,#1556,#1379,.T.);
#1841=EDGE_CURVE('',#1554,#1555,#267,.T.);
#1842=EDGE_CURVE('',#1557,#1557,#1380,.T.);
#1843=EDGE_CURVE('',#1557,#1558,#908,.T.);
#1844=EDGE_CURVE('',#1558,#1558,#1381,.T.);
#1845=EDGE_CURVE('',#1559,#1559,#1382,.T.);
#1846=EDGE_CURVE('',#1559,#1560,#909,.T.);
#1847=EDGE_CURVE('',#1560,#1560,#1383,.T.);
#1848=EDGE_CURVE('',#1561,#1561,#1384,.T.);
#1849=EDGE_CURVE('',#1561,#1562,#910,.T.);
#1850=EDGE_CURVE('',#1562,#1562,#1385,.T.);
#1851=EDGE_CURVE('',#1563,#1563,#1386,.T.);
#1852=EDGE_CURVE('',#1563,#1564,#911,.T.);
#1853=EDGE_CURVE('',#1564,#1564,#1387,.T.);
#1854=EDGE_CURVE('',#1565,#1566,#268,.T.);
#1855=EDGE_CURVE('',#1567,#1565,#269,.T.);
#1856=EDGE_CURVE('',#1567,#1568,#912,.T.);
#1857=EDGE_CURVE('',#1568,#1568,#1388,.T.);
#1858=EDGE_CURVE('',#1566,#1567,#270,.T.);
#1859=EDGE_CURVE('',#1569,#1570,#271,.T.);
#1860=EDGE_CURVE('',#1571,#1569,#272,.T.);
#1861=EDGE_CURVE('',#1571,#1572,#913,.T.);
#1862=EDGE_CURVE('',#1572,#1572,#1389,.T.);
#1863=EDGE_CURVE('',#1570,#1571,#273,.T.);
#1864=EDGE_CURVE('',#1573,#1574,#274,.T.);
#1865=EDGE_CURVE('',#1575,#1573,#275,.T.);
#1866=EDGE_CURVE('',#1575,#1576,#914,.T.);
#1867=EDGE_CURVE('',#1576,#1576,#1390,.T.);
#1868=EDGE_CURVE('',#1574,#1575,#276,.T.);
#1869=EDGE_CURVE('',#1577,#1577,#1391,.T.);
#1870=EDGE_CURVE('',#1577,#1578,#915,.T.);
#1871=EDGE_CURVE('',#1578,#1578,#1392,.T.);
#1872=EDGE_CURVE('',#1579,#1579,#1393,.T.);
#1873=EDGE_CURVE('',#1579,#1580,#916,.T.);
#1874=EDGE_CURVE('',#1580,#1580,#1394,.T.);
#1875=EDGE_CURVE('',#1581,#1581,#1395,.T.);
#1876=EDGE_CURVE('',#1581,#1582,#917,.T.);
#1877=EDGE_CURVE('',#1582,#1582,#1396,.T.);
#1878=EDGE_CURVE('',#1583,#1583,#1397,.T.);
#1879=EDGE_CURVE('',#1583,#1584,#918,.T.);
#1880=EDGE_CURVE('',#1584,#1584,#1398,.T.);
#1881=EDGE_CURVE('',#1585,#1585,#1399,.T.);
#1882=EDGE_CURVE('',#1585,#1586,#919,.T.);
#1883=EDGE_CURVE('',#1586,#1586,#1400,.T.);
#1884=EDGE_CURVE('',#1587,#1587,#1401,.T.);
#1885=EDGE_CURVE('',#1588,#1588,#1402,.T.);
#1886=EDGE_CURVE('',#1588,#1589,#920,.T.);
#1887=EDGE_CURVE('',#1589,#1589,#1403,.T.);
#1888=EDGE_CURVE('',#1590,#1590,#1404,.T.);
#1889=EDGE_CURVE('',#1591,#1591,#1405,.T.);
#1890=EDGE_CURVE('',#1591,#1592,#921,.T.);
#1891=EDGE_CURVE('',#1592,#1592,#1406,.T.);
#1892=EDGE_CURVE('',#1593,#1593,#1407,.T.);
#1893=EDGE_CURVE('',#1594,#1594,#1408,.T.);
#1894=EDGE_CURVE('',#1594,#1595,#922,.T.);
#1895=EDGE_CURVE('',#1595,#1595,#1409,.T.);
#1896=EDGE_CURVE('',#1596,#1596,#1410,.T.);
#1897=EDGE_CURVE('',#1597,#1597,#1411,.T.);
#1898=EDGE_CURVE('',#1597,#1598,#923,.T.);
#1899=EDGE_CURVE('',#1598,#1598,#1412,.T.);
#1900=EDGE_CURVE('',#1599,#1599,#1413,.T.);
#1901=EDGE_CURVE('',#1600,#1600,#1414,.T.);
#1902=EDGE_CURVE('',#1600,#1601,#924,.T.);
#1903=EDGE_CURVE('',#1601,#1601,#1415,.T.);
#1904=EDGE_CURVE('',#1602,#1602,#1416,.T.);
#1905=EDGE_CURVE('',#1596,#1567,#925,.T.);
#1906=EDGE_CURVE('',#1566,#1547,#926,.T.);
#1907=EDGE_CURVE('',#1546,#1587,#927,.T.);
#1908=EDGE_CURVE('',#1599,#1571,#928,.T.);
#1909=EDGE_CURVE('',#1570,#1551,#929,.T.);
#1910=EDGE_CURVE('',#1550,#1590,#930,.T.);
#1911=EDGE_CURVE('',#1602,#1575,#931,.T.);
#1912=EDGE_CURVE('',#1574,#1555,#932,.T.);
#1913=EDGE_CURVE('',#1554,#1593,#933,.T.);
#1914=EDGE_CURVE('',#1603,#1604,#934,.T.);
#1915=EDGE_CURVE('',#1604,#1605,#935,.T.);
#1916=EDGE_CURVE('',#1606,#1605,#936,.T.);
#1917=EDGE_CURVE('',#1603,#1606,#937,.T.);
#1918=EDGE_CURVE('',#1607,#1603,#938,.T.);
#1919=EDGE_CURVE('',#1608,#1606,#939,.T.);
#1920=EDGE_CURVE('',#1607,#1608,#940,.T.);
#1921=EDGE_CURVE('',#1609,#1607,#941,.T.);
#1922=EDGE_CURVE('',#1610,#1608,#942,.T.);
#1923=EDGE_CURVE('',#1609,#1610,#943,.T.);
#1924=EDGE_CURVE('',#1604,#1609,#944,.T.);
#1925=EDGE_CURVE('',#1605,#1610,#945,.T.);
#1926=EDGE_CURVE('',#1611,#1611,#1417,.T.);
#1927=EDGE_CURVE('',#1611,#1612,#946,.T.);
#1928=EDGE_CURVE('',#1612,#1612,#1418,.T.);
#1929=EDGE_CURVE('',#1613,#1613,#1419,.T.);
#1930=EDGE_CURVE('',#1613,#1614,#947,.T.);
#1931=EDGE_CURVE('',#1614,#1614,#1420,.T.);
#1932=EDGE_CURVE('',#1615,#1615,#1421,.T.);
#1933=EDGE_CURVE('',#1615,#1616,#948,.T.);
#1934=EDGE_CURVE('',#1616,#1616,#1422,.T.);
#1935=EDGE_CURVE('',#1617,#1617,#1423,.T.);
#1936=EDGE_CURVE('',#1617,#1618,#949,.T.);
#1937=EDGE_CURVE('',#1618,#1618,#1424,.T.);
#1938=EDGE_CURVE('',#1619,#1619,#1425,.T.);
#1939=EDGE_CURVE('',#1619,#1620,#950,.T.);
#1940=EDGE_CURVE('',#1620,#1620,#1426,.T.);
#1941=EDGE_CURVE('',#1621,#1621,#1427,.T.);
#1942=EDGE_CURVE('',#1621,#1622,#951,.T.);
#1943=EDGE_CURVE('',#1622,#1622,#1428,.T.);
#1944=EDGE_CURVE('',#1623,#1623,#1429,.T.);
#1945=EDGE_CURVE('',#1624,#1624,#1430,.T.);
#1946=EDGE_CURVE('',#1625,#1625,#1431,.T.);
#1947=EDGE_CURVE('',#1626,#1626,#1432,.T.);
#1948=EDGE_CURVE('',#1626,#1624,#952,.T.);
#1949=EDGE_CURVE('',#1625,#1627,#953,.T.);
#1950=EDGE_CURVE('',#1627,#1627,#1433,.T.);
#1951=EDGE_CURVE('',#1623,#1628,#954,.T.);
#1952=EDGE_CURVE('',#1628,#1628,#1434,.T.);
#1953=EDGE_CURVE('',#1629,#1629,#1435,.T.);
#1954=EDGE_CURVE('',#1629,#1630,#955,.T.);
#1955=EDGE_CURVE('',#1630,#1630,#1436,.T.);
#1956=EDGE_CURVE('',#1631,#1631,#1437,.T.);
#1957=EDGE_CURVE('',#1631,#1632,#956,.T.);
#1958=EDGE_CURVE('',#1632,#1632,#1438,.T.);
#1959=EDGE_CURVE('',#1633,#1633,#1439,.T.);
#1960=EDGE_CURVE('',#1633,#1634,#957,.T.);
#1961=EDGE_CURVE('',#1634,#1634,#1440,.T.);
#1962=EDGE_CURVE('',#1635,#1635,#1441,.T.);
#1963=EDGE_CURVE('',#1635,#1636,#958,.T.);
#1964=EDGE_CURVE('',#1636,#1636,#1442,.T.);
#1965=EDGE_CURVE('',#1637,#1637,#1443,.T.);
#1966=EDGE_CURVE('',#1637,#1638,#959,.T.);
#1967=EDGE_CURVE('',#1638,#1638,#1444,.T.);
#1968=EDGE_CURVE('',#1639,#1639,#1445,.T.);
#1969=EDGE_CURVE('',#1639,#1640,#960,.T.);
#1970=EDGE_CURVE('',#1640,#1640,#1446,.T.);
#1971=EDGE_CURVE('',#1641,#1641,#1447,.T.);
#1972=EDGE_CURVE('',#1641,#1642,#961,.T.);
#1973=EDGE_CURVE('',#1642,#1642,#1448,.T.);
#1974=EDGE_CURVE('',#1643,#1643,#1449,.T.);
#1975=EDGE_CURVE('',#1644,#1644,#1450,.T.);
#1976=EDGE_CURVE('',#1645,#1645,#1451,.T.);
#1977=EDGE_CURVE('',#1646,#1646,#1452,.T.);
#1978=EDGE_CURVE('',#1646,#1644,#962,.T.);
#1979=EDGE_CURVE('',#1645,#1647,#963,.T.);
#1980=EDGE_CURVE('',#1647,#1647,#1453,.T.);
#1981=EDGE_CURVE('',#1643,#1648,#964,.T.);
#1982=EDGE_CURVE('',#1648,#1648,#1454,.T.);
#1983=EDGE_CURVE('',#1649,#1649,#1455,.T.);
#1984=EDGE_CURVE('',#1649,#1650,#965,.T.);
#1985=EDGE_CURVE('',#1650,#1650,#1456,.T.);
#1986=EDGE_CURVE('',#1651,#1652,#966,.T.);
#1987=EDGE_CURVE('',#1652,#1653,#967,.T.);
#1988=EDGE_CURVE('',#1653,#1654,#968,.T.);
#1989=EDGE_CURVE('',#1654,#1655,#969,.T.);
#1990=EDGE_CURVE('',#1655,#1656,#970,.T.);
#1991=EDGE_CURVE('',#1656,#1651,#971,.T.);
#1992=EDGE_CURVE('',#1657,#1657,#1457,.T.);
#1993=EDGE_CURVE('',#1658,#1659,#972,.T.);
#1994=EDGE_CURVE('',#1659,#1660,#973,.T.);
#1995=EDGE_CURVE('',#1660,#1661,#974,.T.);
#1996=EDGE_CURVE('',#1661,#1662,#975,.T.);
#1997=EDGE_CURVE('',#1662,#1663,#976,.T.);
#1998=EDGE_CURVE('',#1663,#1658,#977,.T.);
#1999=EDGE_CURVE('',#1664,#1664,#1458,.T.);
#2000=EDGE_CURVE('',#1658,#1652,#978,.T.);
#2001=EDGE_CURVE('',#1653,#1663,#979,.T.);
#2002=EDGE_CURVE('',#1654,#1662,#980,.T.);
#2003=EDGE_CURVE('',#1655,#1661,#981,.T.);
#2004=EDGE_CURVE('',#1656,#1660,#982,.T.);
#2005=EDGE_CURVE('',#1651,#1659,#983,.T.);
#2006=EDGE_CURVE('',#1664,#1665,#984,.T.);
#2007=EDGE_CURVE('',#1665,#1665,#1459,.T.);
#2008=EDGE_CURVE('',#1666,#1666,#1460,.T.);
#2009=EDGE_CURVE('',#1667,#1667,#1461,.T.);
#2010=EDGE_CURVE('',#1665,#1666,#985,.T.);
#2011=EDGE_CURVE('',#1668,#1668,#1462,.T.);
#2012=EDGE_CURVE('',#1668,#1657,#986,.T.);
#2013=EDGE_CURVE('',#1669,#1669,#1463,.T.);
#2014=EDGE_CURVE('',#1669,#1668,#987,.T.);
#2015=EDGE_CURVE('',#1670,#1670,#1464,.T.);
#2016=EDGE_CURVE('',#1670,#1667,#988,.T.);
#2017=EDGE_CURVE('',#1671,#1672,#989,.T.);
#2018=EDGE_CURVE('',#1673,#1671,#990,.T.);
#2019=EDGE_CURVE('',#1674,#1673,#991,.T.);
#2020=EDGE_CURVE('',#1675,#1674,#992,.T.);
#2021=EDGE_CURVE('',#1676,#1675,#993,.T.);
#2022=EDGE_CURVE('',#1672,#1676,#994,.T.);
#2023=EDGE_CURVE('',#1677,#1677,#1465,.T.);
#2024=EDGE_CURVE('',#1671,#1678,#995,.T.);
#2025=EDGE_CURVE('',#1679,#1678,#996,.T.);
#2026=EDGE_CURVE('',#1673,#1679,#997,.T.);
#2027=EDGE_CURVE('',#1680,#1679,#998,.T.);
#2028=EDGE_CURVE('',#1674,#1680,#999,.T.);
#2029=EDGE_CURVE('',#1681,#1680,#1000,.T.);
#2030=EDGE_CURVE('',#1675,#1681,#1001,.T.);
#2031=EDGE_CURVE('',#1682,#1681,#1002,.T.);
#2032=EDGE_CURVE('',#1676,#1682,#1003,.T.);
#2033=EDGE_CURVE('',#1683,#1682,#1004,.T.);
#2034=EDGE_CURVE('',#1672,#1683,#1005,.T.);
#2035=EDGE_CURVE('',#1678,#1683,#1006,.T.);
#2036=EDGE_CURVE('',#1677,#1684,#1007,.T.);
#2037=EDGE_CURVE('',#1684,#1684,#1466,.T.);
#2038=EDGE_CURVE('',#1685,#1686,#1008,.T.);
#2039=EDGE_CURVE('',#1687,#1685,#1009,.T.);
#2040=EDGE_CURVE('',#1688,#1687,#1010,.T.);
#2041=EDGE_CURVE('',#1688,#1686,#1011,.T.);
#2042=EDGE_CURVE('',#1686,#1689,#1012,.T.);
#2043=EDGE_CURVE('',#1690,#1688,#1013,.T.);
#2044=EDGE_CURVE('',#1690,#1689,#1014,.T.);
#2045=EDGE_CURVE('',#1689,#1691,#1015,.T.);
#2046=EDGE_CURVE('',#1692,#1690,#1016,.T.);
#2047=EDGE_CURVE('',#1692,#1691,#1017,.T.);
#2048=EDGE_CURVE('',#1691,#1685,#1018,.T.);
#2049=EDGE_CURVE('',#1687,#1692,#1019,.T.);
#2050=EDGE_CURVE('',#1693,#1693,#1467,.T.);
#2051=EDGE_CURVE('',#1693,#1694,#1020,.T.);
#2052=EDGE_CURVE('',#1694,#1694,#1468,.T.);
#2053=EDGE_CURVE('',#1695,#1695,#1469,.T.);
#2054=EDGE_CURVE('',#1695,#1696,#1021,.T.);
#2055=EDGE_CURVE('',#1696,#1696,#1470,.T.);
#2056=EDGE_CURVE('',#1697,#1697,#1471,.T.);
#2057=EDGE_CURVE('',#1698,#1698,#1472,.T.);
#2058=EDGE_CURVE('',#1698,#1699,#1022,.T.);
#2059=EDGE_CURVE('',#1699,#1699,#1473,.T.);
#2060=EDGE_CURVE('',#1700,#1700,#1474,.T.);
#2061=EDGE_CURVE('',#1701,#1701,#1475,.T.);
#2062=EDGE_CURVE('',#1701,#1702,#1023,.T.);
#2063=EDGE_CURVE('',#1702,#1702,#1476,.T.);
#2064=EDGE_CURVE('',#1703,#1703,#1477,.T.);
#2065=EDGE_CURVE('',#1704,#1704,#1478,.T.);
#2066=EDGE_CURVE('',#1704,#1705,#1024,.T.);
#2067=EDGE_CURVE('',#1705,#1705,#1479,.T.);
#2068=EDGE_CURVE('',#1706,#1706,#1480,.T.);
#2069=EDGE_CURVE('',#1707,#1707,#1481,.T.);
#2070=EDGE_CURVE('',#1707,#1697,#1025,.T.);
#2071=EDGE_CURVE('',#1708,#1708,#1482,.T.);
#2072=EDGE_CURVE('',#1708,#1700,#1026,.T.);
#2073=EDGE_CURVE('',#1709,#1709,#1483,.T.);
#2074=EDGE_CURVE('',#1709,#1703,#1027,.T.);
#2075=EDGE_CURVE('',#1710,#1710,#1484,.T.);
#2076=EDGE_CURVE('',#1710,#1706,#1028,.T.);
#2077=EDGE_CURVE('',#1711,#1711,#1485,.T.);
#2078=EDGE_CURVE('',#1711,#1712,#1029,.T.);
#2079=EDGE_CURVE('',#1712,#1712,#1486,.T.);
#2080=EDGE_CURVE('',#1713,#1713,#1487,.T.);
#2081=EDGE_CURVE('',#1714,#1714,#1488,.T.);
#2082=EDGE_CURVE('',#1714,#1715,#1030,.T.);
#2083=EDGE_CURVE('',#1715,#1715,#1489,.T.);
#2084=EDGE_CURVE('',#1716,#1716,#1490,.T.);
#2085=EDGE_CURVE('',#1716,#1713,#1031,.T.);
#2086=EDGE_CURVE('',#1717,#1717,#1491,.T.);
#2087=EDGE_CURVE('',#1717,#1718,#1032,.T.);
#2088=EDGE_CURVE('',#1718,#1718,#1492,.T.);
#2089=EDGE_CURVE('',#1719,#1720,#1033,.T.);
#2090=EDGE_CURVE('',#1720,#1721,#1034,.T.);
#2091=EDGE_CURVE('',#1722,#1721,#1035,.T.);
#2092=EDGE_CURVE('',#1719,#1722,#1036,.T.);
#2093=EDGE_CURVE('',#1723,#1719,#1037,.T.);
#2094=EDGE_CURVE('',#1724,#1722,#1038,.T.);
#2095=EDGE_CURVE('',#1723,#1724,#1039,.T.);
#2096=EDGE_CURVE('',#1725,#1723,#1040,.T.);
#2097=EDGE_CURVE('',#1726,#1724,#1041,.T.);
#2098=EDGE_CURVE('',#1725,#1726,#1042,.T.);
#2099=EDGE_CURVE('',#1720,#1725,#1043,.T.);
#2100=EDGE_CURVE('',#1721,#1726,#1044,.T.);
#2101=EDGE_CURVE('',#1727,#1727,#1493,.T.);
#2102=EDGE_CURVE('',#1727,#1728,#1045,.T.);
#2103=EDGE_CURVE('',#1728,#1728,#1494,.T.);
#2104=EDGE_CURVE('',#1729,#1729,#1495,.T.);
#2105=EDGE_CURVE('',#1729,#1730,#1046,.T.);
#2106=EDGE_CURVE('',#1730,#1730,#1496,.T.);
#2107=EDGE_CURVE('',#1731,#1731,#1497,.T.);
#2108=EDGE_CURVE('',#1731,#1732,#1047,.T.);
#2109=EDGE_CURVE('',#1732,#1732,#1498,.T.);
#2110=EDGE_CURVE('',#1733,#1733,#1499,.T.);
#2111=EDGE_CURVE('',#1733,#1734,#1048,.T.);
#2112=EDGE_CURVE('',#1734,#1734,#1500,.T.);
#2113=EDGE_CURVE('',#1735,#1735,#1501,.T.);
#2114=EDGE_CURVE('',#1735,#1736,#1049,.T.);
#2115=EDGE_CURVE('',#1736,#1736,#1502,.T.);
#2116=EDGE_CURVE('',#1737,#1737,#1503,.T.);
#2117=EDGE_CURVE('',#1737,#1738,#1050,.T.);
#2118=EDGE_CURVE('',#1738,#1738,#1504,.T.);
#2119=EDGE_CURVE('',#1739,#1739,#1505,.T.);
#2120=EDGE_CURVE('',#1739,#1740,#1051,.T.);
#2121=EDGE_CURVE('',#1740,#1740,#1506,.T.);
#2122=EDGE_CURVE('',#1741,#1742,#1052,.T.);
#2123=EDGE_CURVE('',#1742,#1743,#1053,.T.);
#2124=EDGE_CURVE('',#1744,#1743,#1054,.T.);
#2125=EDGE_CURVE('',#1741,#1744,#1055,.T.);
#2126=EDGE_CURVE('',#1745,#1741,#1056,.T.);
#2127=EDGE_CURVE('',#1746,#1744,#1057,.T.);
#2128=EDGE_CURVE('',#1745,#1746,#1058,.T.);
#2129=EDGE_CURVE('',#1747,#1745,#1059,.T.);
#2130=EDGE_CURVE('',#1748,#1746,#1060,.T.);
#2131=EDGE_CURVE('',#1747,#1748,#1061,.T.);
#2132=EDGE_CURVE('',#1742,#1747,#1062,.T.);
#2133=EDGE_CURVE('',#1743,#1748,#1063,.T.);
#2134=EDGE_CURVE('',#1749,#1749,#1507,.T.);
#2135=EDGE_CURVE('',#1749,#1750,#1064,.T.);
#2136=EDGE_CURVE('',#1750,#1750,#1508,.T.);
#2137=EDGE_CURVE('',#1751,#1751,#1509,.T.);
#2138=EDGE_CURVE('',#1752,#1753,#1065,.T.);
#2139=EDGE_CURVE('',#1754,#1752,#1066,.T.);
#2140=EDGE_CURVE('',#1755,#1754,#1067,.T.);
#2141=EDGE_CURVE('',#1756,#1755,#1068,.T.);
#2142=EDGE_CURVE('',#1757,#1756,#1069,.T.);
#2143=EDGE_CURVE('',#1753,#1757,#1070,.T.);
#2144=EDGE_CURVE('',#1758,#1758,#1510,.T.);
#2145=EDGE_CURVE('',#1752,#1759,#1071,.T.);
#2146=EDGE_CURVE('',#1760,#1759,#1072,.T.);
#2147=EDGE_CURVE('',#1754,#1760,#1073,.T.);
#2148=EDGE_CURVE('',#1761,#1760,#1074,.T.);
#2149=EDGE_CURVE('',#1755,#1761,#1075,.T.);
#2150=EDGE_CURVE('',#1762,#1761,#1076,.T.);
#2151=EDGE_CURVE('',#1756,#1762,#1077,.T.);
#2152=EDGE_CURVE('',#1763,#1762,#1078,.T.);
#2153=EDGE_CURVE('',#1757,#1763,#1079,.T.);
#2154=EDGE_CURVE('',#1764,#1763,#1080,.T.);
#2155=EDGE_CURVE('',#1753,#1764,#1081,.T.);
#2156=EDGE_CURVE('',#1759,#1764,#1082,.T.);
#2157=EDGE_CURVE('',#1751,#1765,#1083,.T.);
#2158=EDGE_CURVE('',#1765,#1765,#1511,.T.);
#2159=EDGE_CURVE('',#1758,#1766,#1084,.T.);
#2160=EDGE_CURVE('',#1766,#1766,#1512,.T.);
#2161=EDGE_CURVE('',#1767,#1767,#1513,.T.);
#2162=EDGE_CURVE('',#1767,#1768,#1085,.T.);
#2163=EDGE_CURVE('',#1768,#1768,#1514,.T.);
#2164=EDGE_CURVE('',#1769,#1769,#1515,.T.);
#2165=EDGE_CURVE('',#1770,#1771,#1086,.T.);
#2166=EDGE_CURVE('',#1771,#1772,#1087,.T.);
#2167=EDGE_CURVE('',#1772,#1773,#1088,.T.);
#2168=EDGE_CURVE('',#1773,#1774,#1089,.T.);
#2169=EDGE_CURVE('',#1774,#1775,#1090,.T.);
#2170=EDGE_CURVE('',#1775,#1770,#1091,.T.);
#2171=EDGE_CURVE('',#1776,#1776,#1516,.T.);
#2172=EDGE_CURVE('',#1777,#1778,#1092,.T.);
#2173=EDGE_CURVE('',#1779,#1777,#1093,.T.);
#2174=EDGE_CURVE('',#1780,#1779,#1094,.T.);
#2175=EDGE_CURVE('',#1781,#1780,#1095,.T.);
#2176=EDGE_CURVE('',#1782,#1781,#1096,.T.);
#2177=EDGE_CURVE('',#1778,#1782,#1097,.T.);
#2178=EDGE_CURVE('',#1783,#1783,#1517,.T.);
#2179=EDGE_CURVE('',#1777,#1770,#1098,.T.);
#2180=EDGE_CURVE('',#1779,#1775,#1099,.T.);
#2181=EDGE_CURVE('',#1780,#1774,#1100,.T.);
#2182=EDGE_CURVE('',#1781,#1773,#1101,.T.);
#2183=EDGE_CURVE('',#1782,#1772,#1102,.T.);
#2184=EDGE_CURVE('',#1778,#1771,#1103,.T.);
#2185=EDGE_CURVE('',#1784,#1784,#1518,.T.);
#2186=EDGE_CURVE('',#1784,#1785,#1104,.T.);
#2187=EDGE_CURVE('',#1785,#1785,#1519,.T.);
#2188=EDGE_CURVE('',#1786,#1786,#1520,.T.);
#2189=EDGE_CURVE('',#1776,#1786,#1105,.T.);
#2190=EDGE_CURVE('',#1787,#1787,#1521,.T.);
#2191=EDGE_CURVE('',#1787,#1783,#1106,.T.);
#2192=EDGE_CURVE('',#1788,#1788,#1522,.T.);
#2193=EDGE_CURVE('',#1788,#1769,#1107,.T.);
#2194=EDGE_CURVE('',#1789,#1789,#1523,.T.);
#2195=EDGE_CURVE('',#1790,#1790,#1524,.T.);
#2196=EDGE_CURVE('',#1791,#1791,#1525,.T.);
#2197=EDGE_CURVE('',#1791,#1789,#1108,.T.);
#2198=EDGE_CURVE('',#1792,#1792,#1526,.T.);
#2199=EDGE_CURVE('',#1793,#1793,#1527,.T.);
#2200=EDGE_CURVE('',#1793,#1792,#1109,.T.);
#2201=EDGE_CURVE('',#1794,#1794,#1528,.T.);
#2202=EDGE_CURVE('',#1794,#1790,#1110,.T.);
#2203=EDGE_CURVE('',#1795,#1795,#1529,.T.);
#2204=EDGE_CURVE('',#1796,#1796,#1530,.T.);
#2205=EDGE_CURVE('',#1796,#1795,#1111,.T.);
#2206=EDGE_CURVE('',#1797,#1797,#1531,.T.);
#2207=EDGE_CURVE('',#1797,#1796,#1112,.T.);
#2208=EDGE_CURVE('',#1798,#1798,#1532,.T.);
#2209=EDGE_CURVE('',#1798,#1797,#1113,.T.);
#2210=EDGE_CURVE('',#1799,#1799,#1533,.T.);
#2211=EDGE_CURVE('',#1800,#1800,#1534,.F.);
#2212=EDGE_CURVE('',#1800,#1799,#1114,.T.);
#2213=EDGE_CURVE('',#1801,#1801,#1535,.F.);
#2214=EDGE_CURVE('',#1801,#1800,#1115,.T.);
#2215=EDGE_CURVE('',#1802,#1802,#1536,.T.);
#2216=EDGE_CURVE('',#1802,#1801,#1116,.T.);
#2217=EDGE_CURVE('',#1803,#1804,#1117,.T.);
#2218=EDGE_CURVE('',#1804,#1805,#1118,.T.);
#2219=EDGE_CURVE('',#1805,#1806,#1119,.T.);
#2220=EDGE_CURVE('',#1803,#1806,#1120,.T.);
#2221=EDGE_CURVE('',#1804,#1807,#1121,.T.);
#2222=EDGE_CURVE('',#1807,#1808,#1122,.T.);
#2223=EDGE_CURVE('',#1808,#1805,#1123,.T.);
#2224=EDGE_CURVE('',#1807,#1809,#1124,.T.);
#2225=EDGE_CURVE('',#1809,#1810,#1125,.T.);
#2226=EDGE_CURVE('',#1810,#1808,#1126,.T.);
#2227=EDGE_CURVE('',#1809,#1811,#1127,.T.);
#2228=EDGE_CURVE('',#1811,#1812,#1128,.T.);
#2229=EDGE_CURVE('',#1812,#1810,#1129,.T.);
#2230=EDGE_CURVE('',#1811,#1813,#1130,.T.);
#2231=EDGE_CURVE('',#1813,#1814,#1131,.T.);
#2232=EDGE_CURVE('',#1814,#1812,#1132,.T.);
#2233=EDGE_CURVE('',#1813,#1803,#1133,.T.);
#2234=EDGE_CURVE('',#1806,#1814,#1134,.T.);
#2235=ORIENTED_EDGE('',*,*,#1815,.F.);
#2236=ORIENTED_EDGE('',*,*,#1816,.T.);
#2237=ORIENTED_EDGE('',*,*,#1817,.F.);
#2238=ORIENTED_EDGE('',*,*,#1816,.F.);
#2239=ORIENTED_EDGE('',*,*,#1815,.T.);
#2240=ORIENTED_EDGE('',*,*,#1818,.F.);
#2241=ORIENTED_EDGE('',*,*,#1819,.T.);
#2242=ORIENTED_EDGE('',*,*,#1820,.F.);
#2243=ORIENTED_EDGE('',*,*,#1819,.F.);
#2244=ORIENTED_EDGE('',*,*,#1818,.T.);
#2245=ORIENTED_EDGE('',*,*,#1821,.F.);
#2246=ORIENTED_EDGE('',*,*,#1822,.T.);
#2247=ORIENTED_EDGE('',*,*,#1823,.F.);
#2248=ORIENTED_EDGE('',*,*,#1822,.F.);
#2249=ORIENTED_EDGE('',*,*,#1821,.T.);
#2250=ORIENTED_EDGE('',*,*,#1824,.F.);
#2251=ORIENTED_EDGE('',*,*,#1825,.T.);
#2252=ORIENTED_EDGE('',*,*,#1826,.F.);
#2253=ORIENTED_EDGE('',*,*,#1825,.F.);
#2254=ORIENTED_EDGE('',*,*,#1824,.T.);
#2255=ORIENTED_EDGE('',*,*,#1827,.F.);
#2256=ORIENTED_EDGE('',*,*,#1828,.F.);
#2257=ORIENTED_EDGE('',*,*,#1829,.T.);
#2258=ORIENTED_EDGE('',*,*,#1830,.F.);
#2259=ORIENTED_EDGE('',*,*,#1829,.F.);
#2260=ORIENTED_EDGE('',*,*,#1831,.F.);
#2261=ORIENTED_EDGE('',*,*,#1832,.F.);
#2262=ORIENTED_EDGE('',*,*,#1833,.F.);
#2263=ORIENTED_EDGE('',*,*,#1834,.T.);
#2264=ORIENTED_EDGE('',*,*,#1835,.F.);
#2265=ORIENTED_EDGE('',*,*,#1834,.F.);
#2266=ORIENTED_EDGE('',*,*,#1836,.F.);
#2267=ORIENTED_EDGE('',*,*,#1837,.F.);
#2268=ORIENTED_EDGE('',*,*,#1838,.F.);
#2269=ORIENTED_EDGE('',*,*,#1839,.T.);
#2270=ORIENTED_EDGE('',*,*,#1840,.F.);
#2271=ORIENTED_EDGE('',*,*,#1839,.F.);
#2272=ORIENTED_EDGE('',*,*,#1841,.F.);
#2273=ORIENTED_EDGE('',*,*,#1842,.F.);
#2274=ORIENTED_EDGE('',*,*,#1843,.T.);
#2275=ORIENTED_EDGE('',*,*,#1844,.F.);
#2276=ORIENTED_EDGE('',*,*,#1843,.F.);
#2277=ORIENTED_EDGE('',*,*,#1842,.T.);
#2278=ORIENTED_EDGE('',*,*,#1845,.F.);
#2279=ORIENTED_EDGE('',*,*,#1846,.T.);
#2280=ORIENTED_EDGE('',*,*,#1847,.F.);
#2281=ORIENTED_EDGE('',*,*,#1846,.F.);
#2282=ORIENTED_EDGE('',*,*,#1845,.T.);
#2283=ORIENTED_EDGE('',*,*,#1848,.F.);
#2284=ORIENTED_EDGE('',*,*,#1849,.T.);
#2285=ORIENTED_EDGE('',*,*,#1850,.F.);
#2286=ORIENTED_EDGE('',*,*,#1849,.F.);
#2287=ORIENTED_EDGE('',*,*,#1848,.T.);
#2288=ORIENTED_EDGE('',*,*,#1851,.F.);
#2289=ORIENTED_EDGE('',*,*,#1852,.T.);
#2290=ORIENTED_EDGE('',*,*,#1853,.F.);
#2291=ORIENTED_EDGE('',*,*,#1852,.F.);
#2292=ORIENTED_EDGE('',*,*,#1851,.T.);
#2293=ORIENTED_EDGE('',*,*,#1854,.F.);
#2294=ORIENTED_EDGE('',*,*,#1855,.F.);
#2295=ORIENTED_EDGE('',*,*,#1856,.T.);
#2296=ORIENTED_EDGE('',*,*,#1857,.F.);
#2297=ORIENTED_EDGE('',*,*,#1856,.F.);
#2298=ORIENTED_EDGE('',*,*,#1858,.F.);
#2299=ORIENTED_EDGE('',*,*,#1859,.F.);
#2300=ORIENTED_EDGE('',*,*,#1860,.F.);
#2301=ORIENTED_EDGE('',*,*,#1861,.T.);
#2302=ORIENTED_EDGE('',*,*,#1862,.F.);
#2303=ORIENTED_EDGE('',*,*,#1861,.F.);
#2304=ORIENTED_EDGE('',*,*,#1863,.F.);
#2305=ORIENTED_EDGE('',*,*,#1864,.F.);
#2306=ORIENTED_EDGE('',*,*,#1865,.F.);
#2307=ORIENTED_EDGE('',*,*,#1866,.T.);
#2308=ORIENTED_EDGE('',*,*,#1867,.F.);
#2309=ORIENTED_EDGE('',*,*,#1866,.F.);
#2310=ORIENTED_EDGE('',*,*,#1868,.F.);
#2311=ORIENTED_EDGE('',*,*,#1869,.F.);
#2312=ORIENTED_EDGE('',*,*,#1870,.T.);
#2313=ORIENTED_EDGE('',*,*,#1871,.F.);
#2314=ORIENTED_EDGE('',*,*,#1870,.F.);
#2315=ORIENTED_EDGE('',*,*,#1872,.F.);
#2316=ORIENTED_EDGE('',*,*,#1873,.T.);
#2317=ORIENTED_EDGE('',*,*,#1874,.F.);
#2318=ORIENTED_EDGE('',*,*,#1873,.F.);
#2319=ORIENTED_EDGE('',*,*,#1875,.F.);
#2320=ORIENTED_EDGE('',*,*,#1876,.T.);
#2321=ORIENTED_EDGE('',*,*,#1877,.F.);
#2322=ORIENTED_EDGE('',*,*,#1876,.F.);
#2323=ORIENTED_EDGE('',*,*,#1878,.F.);
#2324=ORIENTED_EDGE('',*,*,#1879,.T.);
#2325=ORIENTED_EDGE('',*,*,#1880,.F.);
#2326=ORIENTED_EDGE('',*,*,#1879,.F.);
#2327=ORIENTED_EDGE('',*,*,#1881,.F.);
#2328=ORIENTED_EDGE('',*,*,#1882,.T.);
#2329=ORIENTED_EDGE('',*,*,#1883,.F.);
#2330=ORIENTED_EDGE('',*,*,#1882,.F.);
#2331=ORIENTED_EDGE('',*,*,#1881,.T.);
#2332=ORIENTED_EDGE('',*,*,#1884,.F.);
#2333=ORIENTED_EDGE('',*,*,#1885,.F.);
#2334=ORIENTED_EDGE('',*,*,#1886,.T.);
#2335=ORIENTED_EDGE('',*,*,#1887,.F.);
#2336=ORIENTED_EDGE('',*,*,#1886,.F.);
#2337=ORIENTED_EDGE('',*,*,#1885,.T.);
#2338=ORIENTED_EDGE('',*,*,#1888,.F.);
#2339=ORIENTED_EDGE('',*,*,#1889,.F.);
#2340=ORIENTED_EDGE('',*,*,#1890,.T.);
#2341=ORIENTED_EDGE('',*,*,#1891,.F.);
#2342=ORIENTED_EDGE('',*,*,#1890,.F.);
#2343=ORIENTED_EDGE('',*,*,#1889,.T.);
#2344=ORIENTED_EDGE('',*,*,#1892,.F.);
#2345=ORIENTED_EDGE('',*,*,#1893,.F.);
#2346=ORIENTED_EDGE('',*,*,#1894,.T.);
#2347=ORIENTED_EDGE('',*,*,#1895,.T.);
#2348=ORIENTED_EDGE('',*,*,#1894,.F.);
#2349=ORIENTED_EDGE('',*,*,#1895,.F.);
#2350=ORIENTED_EDGE('',*,*,#1896,.F.);
#2351=ORIENTED_EDGE('',*,*,#1897,.F.);
#2352=ORIENTED_EDGE('',*,*,#1898,.T.);
#2353=ORIENTED_EDGE('',*,*,#1899,.T.);
#2354=ORIENTED_EDGE('',*,*,#1898,.F.);
#2355=ORIENTED_EDGE('',*,*,#1899,.F.);
#2356=ORIENTED_EDGE('',*,*,#1900,.F.);
#2357=ORIENTED_EDGE('',*,*,#1901,.F.);
#2358=ORIENTED_EDGE('',*,*,#1902,.T.);
#2359=ORIENTED_EDGE('',*,*,#1903,.T.);
#2360=ORIENTED_EDGE('',*,*,#1902,.F.);
#2361=ORIENTED_EDGE('',*,*,#1903,.F.);
#2362=ORIENTED_EDGE('',*,*,#1904,.F.);
#2363=ORIENTED_EDGE('',*,*,#1896,.T.);
#2364=ORIENTED_EDGE('',*,*,#1905,.T.);
#2365=ORIENTED_EDGE('',*,*,#1855,.T.);
#2366=ORIENTED_EDGE('',*,*,#1854,.T.);
#2367=ORIENTED_EDGE('',*,*,#1906,.T.);
#2368=ORIENTED_EDGE('',*,*,#1828,.T.);
#2369=ORIENTED_EDGE('',*,*,#1827,.T.);
#2370=ORIENTED_EDGE('',*,*,#1907,.T.);
#2371=ORIENTED_EDGE('',*,*,#1884,.T.);
#2372=ORIENTED_EDGE('',*,*,#1907,.F.);
#2373=ORIENTED_EDGE('',*,*,#1831,.T.);
#2374=ORIENTED_EDGE('',*,*,#1906,.F.);
#2375=ORIENTED_EDGE('',*,*,#1858,.T.);
#2376=ORIENTED_EDGE('',*,*,#1905,.F.);
#2377=ORIENTED_EDGE('',*,*,#1900,.T.);
#2378=ORIENTED_EDGE('',*,*,#1908,.T.);
#2379=ORIENTED_EDGE('',*,*,#1860,.T.);
#2380=ORIENTED_EDGE('',*,*,#1859,.T.);
#2381=ORIENTED_EDGE('',*,*,#1909,.T.);
#2382=ORIENTED_EDGE('',*,*,#1833,.T.);
#2383=ORIENTED_EDGE('',*,*,#1832,.T.);
#2384=ORIENTED_EDGE('',*,*,#1910,.T.);
#2385=ORIENTED_EDGE('',*,*,#1888,.T.);
#2386=ORIENTED_EDGE('',*,*,#1910,.F.);
#2387=ORIENTED_EDGE('',*,*,#1836,.T.);
#2388=ORIENTED_EDGE('',*,*,#1909,.F.);
#2389=ORIENTED_EDGE('',*,*,#1863,.T.);
#2390=ORIENTED_EDGE('',*,*,#1908,.F.);
#2391=ORIENTED_EDGE('',*,*,#1904,.T.);
#2392=ORIENTED_EDGE('',*,*,#1911,.T.);
#2393=ORIENTED_EDGE('',*,*,#1865,.T.);
#2394=ORIENTED_EDGE('',*,*,#1864,.T.);
#2395=ORIENTED_EDGE('',*,*,#1912,.T.);
#2396=ORIENTED_EDGE('',*,*,#1838,.T.);
#2397=ORIENTED_EDGE('',*,*,#1837,.T.);
#2398=ORIENTED_EDGE('',*,*,#1913,.T.);
#2399=ORIENTED_EDGE('',*,*,#1892,.T.);
#2400=ORIENTED_EDGE('',*,*,#1913,.F.);
#2401=ORIENTED_EDGE('',*,*,#1841,.T.);
#2402=ORIENTED_EDGE('',*,*,#1912,.F.);
#2403=ORIENTED_EDGE('',*,*,#1868,.T.);
#2404=ORIENTED_EDGE('',*,*,#1911,.F.);
#2405=ORIENTED_EDGE('',*,*,#1914,.T.);
#2406=ORIENTED_EDGE('',*,*,#1915,.T.);
#2407=ORIENTED_EDGE('',*,*,#1916,.F.);
#2408=ORIENTED_EDGE('',*,*,#1917,.F.);
#2409=ORIENTED_EDGE('',*,*,#1918,.T.);
#2410=ORIENTED_EDGE('',*,*,#1917,.T.);
#2411=ORIENTED_EDGE('',*,*,#1919,.F.);
#2412=ORIENTED_EDGE('',*,*,#1920,.F.);
#2413=ORIENTED_EDGE('',*,*,#1891,.T.);
#2414=ORIENTED_EDGE('',*,*,#1887,.T.);
#2415=ORIENTED_EDGE('',*,*,#1883,.T.);
#2416=ORIENTED_EDGE('',*,*,#1921,.T.);
#2417=ORIENTED_EDGE('',*,*,#1920,.T.);
#2418=ORIENTED_EDGE('',*,*,#1922,.F.);
#2419=ORIENTED_EDGE('',*,*,#1923,.F.);
#2420=ORIENTED_EDGE('',*,*,#1924,.T.);
#2421=ORIENTED_EDGE('',*,*,#1923,.T.);
#2422=ORIENTED_EDGE('',*,*,#1925,.F.);
#2423=ORIENTED_EDGE('',*,*,#1915,.F.);
#2424=ORIENTED_EDGE('',*,*,#1901,.T.);
#2425=ORIENTED_EDGE('',*,*,#1897,.T.);
#2426=ORIENTED_EDGE('',*,*,#1893,.T.);
#2427=ORIENTED_EDGE('',*,*,#1925,.T.);
#2428=ORIENTED_EDGE('',*,*,#1922,.T.);
#2429=ORIENTED_EDGE('',*,*,#1919,.T.);
#2430=ORIENTED_EDGE('',*,*,#1916,.T.);
#2431=ORIENTED_EDGE('',*,*,#1830,.T.);
#2432=ORIENTED_EDGE('',*,*,#1835,.T.);
#2433=ORIENTED_EDGE('',*,*,#1840,.T.);
#2434=ORIENTED_EDGE('',*,*,#1857,.T.);
#2435=ORIENTED_EDGE('',*,*,#1862,.T.);
#2436=ORIENTED_EDGE('',*,*,#1867,.T.);
#2437=ORIENTED_EDGE('',*,*,#1871,.T.);
#2438=ORIENTED_EDGE('',*,*,#1874,.T.);
#2439=ORIENTED_EDGE('',*,*,#1877,.T.);
#2440=ORIENTED_EDGE('',*,*,#1880,.T.);
#2441=ORIENTED_EDGE('',*,*,#1853,.T.);
#2442=ORIENTED_EDGE('',*,*,#1850,.T.);
#2443=ORIENTED_EDGE('',*,*,#1847,.T.);
#2444=ORIENTED_EDGE('',*,*,#1844,.T.);
#2445=ORIENTED_EDGE('',*,*,#1826,.T.);
#2446=ORIENTED_EDGE('',*,*,#1823,.T.);
#2447=ORIENTED_EDGE('',*,*,#1820,.T.);
#2448=ORIENTED_EDGE('',*,*,#1817,.T.);
#2449=ORIENTED_EDGE('',*,*,#1924,.F.);
#2450=ORIENTED_EDGE('',*,*,#1914,.F.);
#2451=ORIENTED_EDGE('',*,*,#1918,.F.);
#2452=ORIENTED_EDGE('',*,*,#1921,.F.);
#2453=ORIENTED_EDGE('',*,*,#1869,.T.);
#2454=ORIENTED_EDGE('',*,*,#1872,.T.);
#2455=ORIENTED_EDGE('',*,*,#1875,.T.);
#2456=ORIENTED_EDGE('',*,*,#1878,.T.);
#2457=ORIENTED_EDGE('',*,*,#1926,.F.);
#2458=ORIENTED_EDGE('',*,*,#1927,.T.);
#2459=ORIENTED_EDGE('',*,*,#1928,.F.);
#2460=ORIENTED_EDGE('',*,*,#1927,.F.);
#2461=ORIENTED_EDGE('',*,*,#1929,.F.);
#2462=ORIENTED_EDGE('',*,*,#1930,.T.);
#2463=ORIENTED_EDGE('',*,*,#1931,.F.);
#2464=ORIENTED_EDGE('',*,*,#1930,.F.);
#2465=ORIENTED_EDGE('',*,*,#1932,.F.);
#2466=ORIENTED_EDGE('',*,*,#1933,.T.);
#2467=ORIENTED_EDGE('',*,*,#1934,.F.);
#2468=ORIENTED_EDGE('',*,*,#1933,.F.);
#2469=ORIENTED_EDGE('',*,*,#1935,.F.);
#2470=ORIENTED_EDGE('',*,*,#1936,.T.);
#2471=ORIENTED_EDGE('',*,*,#1937,.F.);
#2472=ORIENTED_EDGE('',*,*,#1936,.F.);
#2473=ORIENTED_EDGE('',*,*,#1938,.F.);
#2474=ORIENTED_EDGE('',*,*,#1939,.T.);
#2475=ORIENTED_EDGE('',*,*,#1940,.F.);
#2476=ORIENTED_EDGE('',*,*,#1939,.F.);
#2477=ORIENTED_EDGE('',*,*,#1941,.F.);
#2478=ORIENTED_EDGE('',*,*,#1942,.T.);
#2479=ORIENTED_EDGE('',*,*,#1943,.F.);
#2480=ORIENTED_EDGE('',*,*,#1942,.F.);
#2481=ORIENTED_EDGE('',*,*,#1944,.F.);
#2482=ORIENTED_EDGE('',*,*,#1941,.T.);
#2483=ORIENTED_EDGE('',*,*,#1938,.T.);
#2484=ORIENTED_EDGE('',*,*,#1935,.T.);
#2485=ORIENTED_EDGE('',*,*,#1932,.T.);
#2486=ORIENTED_EDGE('',*,*,#1929,.T.);
#2487=ORIENTED_EDGE('',*,*,#1926,.T.);
#2488=ORIENTED_EDGE('',*,*,#1945,.F.);
#2489=ORIENTED_EDGE('',*,*,#1946,.F.);
#2490=ORIENTED_EDGE('',*,*,#1947,.F.);
#2491=ORIENTED_EDGE('',*,*,#1948,.T.);
#2492=ORIENTED_EDGE('',*,*,#1945,.T.);
#2493=ORIENTED_EDGE('',*,*,#1948,.F.);
#2494=ORIENTED_EDGE('',*,*,#1947,.T.);
#2495=ORIENTED_EDGE('',*,*,#1943,.T.);
#2496=ORIENTED_EDGE('',*,*,#1940,.T.);
#2497=ORIENTED_EDGE('',*,*,#1937,.T.);
#2498=ORIENTED_EDGE('',*,*,#1934,.T.);
#2499=ORIENTED_EDGE('',*,*,#1931,.T.);
#2500=ORIENTED_EDGE('',*,*,#1928,.T.);
#2501=ORIENTED_EDGE('',*,*,#1946,.T.);
#2502=ORIENTED_EDGE('',*,*,#1949,.T.);
#2503=ORIENTED_EDGE('',*,*,#1950,.F.);
#2504=ORIENTED_EDGE('',*,*,#1949,.F.);
#2505=ORIENTED_EDGE('',*,*,#1944,.T.);
#2506=ORIENTED_EDGE('',*,*,#1951,.T.);
#2507=ORIENTED_EDGE('',*,*,#1952,.T.);
#2508=ORIENTED_EDGE('',*,*,#1951,.F.);
#2509=ORIENTED_EDGE('',*,*,#1953,.F.);
#2510=ORIENTED_EDGE('',*,*,#1954,.T.);
#2511=ORIENTED_EDGE('',*,*,#1955,.T.);
#2512=ORIENTED_EDGE('',*,*,#1954,.F.);
#2513=ORIENTED_EDGE('',*,*,#1953,.T.);
#2514=ORIENTED_EDGE('',*,*,#1950,.T.);
#2515=ORIENTED_EDGE('',*,*,#1955,.F.);
#2516=ORIENTED_EDGE('',*,*,#1952,.F.);
#2517=ORIENTED_EDGE('',*,*,#1956,.F.);
#2518=ORIENTED_EDGE('',*,*,#1957,.T.);
#2519=ORIENTED_EDGE('',*,*,#1958,.F.);
#2520=ORIENTED_EDGE('',*,*,#1957,.F.);
#2521=ORIENTED_EDGE('',*,*,#1959,.F.);
#2522=ORIENTED_EDGE('',*,*,#1960,.T.);
#2523=ORIENTED_EDGE('',*,*,#1961,.F.);
#2524=ORIENTED_EDGE('',*,*,#1960,.F.);
#2525=ORIENTED_EDGE('',*,*,#1962,.F.);
#2526=ORIENTED_EDGE('',*,*,#1963,.T.);
#2527=ORIENTED_EDGE('',*,*,#1964,.F.);
#2528=ORIENTED_EDGE('',*,*,#1963,.F.);
#2529=ORIENTED_EDGE('',*,*,#1965,.F.);
#2530=ORIENTED_EDGE('',*,*,#1966,.T.);
#2531=ORIENTED_EDGE('',*,*,#1967,.F.);
#2532=ORIENTED_EDGE('',*,*,#1966,.F.);
#2533=ORIENTED_EDGE('',*,*,#1968,.F.);
#2534=ORIENTED_EDGE('',*,*,#1969,.T.);
#2535=ORIENTED_EDGE('',*,*,#1970,.F.);
#2536=ORIENTED_EDGE('',*,*,#1969,.F.);
#2537=ORIENTED_EDGE('',*,*,#1971,.F.);
#2538=ORIENTED_EDGE('',*,*,#1972,.T.);
#2539=ORIENTED_EDGE('',*,*,#1973,.F.);
#2540=ORIENTED_EDGE('',*,*,#1972,.F.);
#2541=ORIENTED_EDGE('',*,*,#1974,.F.);
#2542=ORIENTED_EDGE('',*,*,#1971,.T.);
#2543=ORIENTED_EDGE('',*,*,#1968,.T.);
#2544=ORIENTED_EDGE('',*,*,#1965,.T.);
#2545=ORIENTED_EDGE('',*,*,#1962,.T.);
#2546=ORIENTED_EDGE('',*,*,#1959,.T.);
#2547=ORIENTED_EDGE('',*,*,#1956,.T.);
#2548=ORIENTED_EDGE('',*,*,#1975,.F.);
#2549=ORIENTED_EDGE('',*,*,#1976,.F.);
#2550=ORIENTED_EDGE('',*,*,#1977,.F.);
#2551=ORIENTED_EDGE('',*,*,#1978,.T.);
#2552=ORIENTED_EDGE('',*,*,#1975,.T.);
#2553=ORIENTED_EDGE('',*,*,#1978,.F.);
#2554=ORIENTED_EDGE('',*,*,#1977,.T.);
#2555=ORIENTED_EDGE('',*,*,#1973,.T.);
#2556=ORIENTED_EDGE('',*,*,#1970,.T.);
#2557=ORIENTED_EDGE('',*,*,#1967,.T.);
#2558=ORIENTED_EDGE('',*,*,#1964,.T.);
#2559=ORIENTED_EDGE('',*,*,#1961,.T.);
#2560=ORIENTED_EDGE('',*,*,#1958,.T.);
#2561=ORIENTED_EDGE('',*,*,#1976,.T.);
#2562=ORIENTED_EDGE('',*,*,#1979,.T.);
#2563=ORIENTED_EDGE('',*,*,#1980,.F.);
#2564=ORIENTED_EDGE('',*,*,#1979,.F.);
#2565=ORIENTED_EDGE('',*,*,#1974,.T.);
#2566=ORIENTED_EDGE('',*,*,#1981,.T.);
#2567=ORIENTED_EDGE('',*,*,#1982,.T.);
#2568=ORIENTED_EDGE('',*,*,#1981,.F.);
#2569=ORIENTED_EDGE('',*,*,#1983,.F.);
#2570=ORIENTED_EDGE('',*,*,#1984,.T.);
#2571=ORIENTED_EDGE('',*,*,#1985,.T.);
#2572=ORIENTED_EDGE('',*,*,#1984,.F.);
#2573=ORIENTED_EDGE('',*,*,#1983,.T.);
#2574=ORIENTED_EDGE('',*,*,#1980,.T.);
#2575=ORIENTED_EDGE('',*,*,#1985,.F.);
#2576=ORIENTED_EDGE('',*,*,#1982,.F.);
#2577=ORIENTED_EDGE('',*,*,#1986,.T.);
#2578=ORIENTED_EDGE('',*,*,#1987,.T.);
#2579=ORIENTED_EDGE('',*,*,#1988,.T.);
#2580=ORIENTED_EDGE('',*,*,#1989,.T.);
#2581=ORIENTED_EDGE('',*,*,#1990,.T.);
#2582=ORIENTED_EDGE('',*,*,#1991,.T.);
#2583=ORIENTED_EDGE('',*,*,#1992,.F.);
#2584=ORIENTED_EDGE('',*,*,#1993,.T.);
#2585=ORIENTED_EDGE('',*,*,#1994,.T.);
#2586=ORIENTED_EDGE('',*,*,#1995,.T.);
#2587=ORIENTED_EDGE('',*,*,#1996,.T.);
#2588=ORIENTED_EDGE('',*,*,#1997,.T.);
#2589=ORIENTED_EDGE('',*,*,#1998,.T.);
#2590=ORIENTED_EDGE('',*,*,#1999,.F.);
#2591=ORIENTED_EDGE('',*,*,#2000,.F.);
#2592=ORIENTED_EDGE('',*,*,#1998,.F.);
#2593=ORIENTED_EDGE('',*,*,#2001,.F.);
#2594=ORIENTED_EDGE('',*,*,#1987,.F.);
#2595=ORIENTED_EDGE('',*,*,#2001,.T.);
#2596=ORIENTED_EDGE('',*,*,#1997,.F.);
#2597=ORIENTED_EDGE('',*,*,#2002,.F.);
#2598=ORIENTED_EDGE('',*,*,#1988,.F.);
#2599=ORIENTED_EDGE('',*,*,#2002,.T.);
#2600=ORIENTED_EDGE('',*,*,#1996,.F.);
#2601=ORIENTED_EDGE('',*,*,#2003,.F.);
#2602=ORIENTED_EDGE('',*,*,#1989,.F.);
#2603=ORIENTED_EDGE('',*,*,#2003,.T.);
#2604=ORIENTED_EDGE('',*,*,#1995,.F.);
#2605=ORIENTED_EDGE('',*,*,#2004,.F.);
#2606=ORIENTED_EDGE('',*,*,#1990,.F.);
#2607=ORIENTED_EDGE('',*,*,#2004,.T.);
#2608=ORIENTED_EDGE('',*,*,#1994,.F.);
#2609=ORIENTED_EDGE('',*,*,#2005,.F.);
#2610=ORIENTED_EDGE('',*,*,#1991,.F.);
#2611=ORIENTED_EDGE('',*,*,#2005,.T.);
#2612=ORIENTED_EDGE('',*,*,#1993,.F.);
#2613=ORIENTED_EDGE('',*,*,#2000,.T.);
#2614=ORIENTED_EDGE('',*,*,#1986,.F.);
#2615=ORIENTED_EDGE('',*,*,#1999,.T.);
#2616=ORIENTED_EDGE('',*,*,#2006,.T.);
#2617=ORIENTED_EDGE('',*,*,#2007,.T.);
#2618=ORIENTED_EDGE('',*,*,#2006,.F.);
#2619=ORIENTED_EDGE('',*,*,#2008,.F.);
#2620=ORIENTED_EDGE('',*,*,#2009,.T.);
#2621=ORIENTED_EDGE('',*,*,#2007,.F.);
#2622=ORIENTED_EDGE('',*,*,#2010,.T.);
#2623=ORIENTED_EDGE('',*,*,#2008,.T.);
#2624=ORIENTED_EDGE('',*,*,#2010,.F.);
#2625=ORIENTED_EDGE('',*,*,#2011,.F.);
#2626=ORIENTED_EDGE('',*,*,#2012,.T.);
#2627=ORIENTED_EDGE('',*,*,#1992,.T.);
#2628=ORIENTED_EDGE('',*,*,#2012,.F.);
#2629=ORIENTED_EDGE('',*,*,#2013,.F.);
#2630=ORIENTED_EDGE('',*,*,#2014,.T.);
#2631=ORIENTED_EDGE('',*,*,#2011,.T.);
#2632=ORIENTED_EDGE('',*,*,#2014,.F.);
#2633=ORIENTED_EDGE('',*,*,#2013,.T.);
#2634=ORIENTED_EDGE('',*,*,#2015,.F.);
#2635=ORIENTED_EDGE('',*,*,#2015,.T.);
#2636=ORIENTED_EDGE('',*,*,#2016,.T.);
#2637=ORIENTED_EDGE('',*,*,#2009,.F.);
#2638=ORIENTED_EDGE('',*,*,#2016,.F.);
#2639=ORIENTED_EDGE('',*,*,#2017,.F.);
#2640=ORIENTED_EDGE('',*,*,#2018,.F.);
#2641=ORIENTED_EDGE('',*,*,#2019,.F.);
#2642=ORIENTED_EDGE('',*,*,#2020,.F.);
#2643=ORIENTED_EDGE('',*,*,#2021,.F.);
#2644=ORIENTED_EDGE('',*,*,#2022,.F.);
#2645=ORIENTED_EDGE('',*,*,#2023,.T.);
#2646=ORIENTED_EDGE('',*,*,#2018,.T.);
#2647=ORIENTED_EDGE('',*,*,#2024,.T.);
#2648=ORIENTED_EDGE('',*,*,#2025,.F.);
#2649=ORIENTED_EDGE('',*,*,#2026,.F.);
#2650=ORIENTED_EDGE('',*,*,#2019,.T.);
#2651=ORIENTED_EDGE('',*,*,#2026,.T.);
#2652=ORIENTED_EDGE('',*,*,#2027,.F.);
#2653=ORIENTED_EDGE('',*,*,#2028,.F.);
#2654=ORIENTED_EDGE('',*,*,#2020,.T.);
#2655=ORIENTED_EDGE('',*,*,#2028,.T.);
#2656=ORIENTED_EDGE('',*,*,#2029,.F.);
#2657=ORIENTED_EDGE('',*,*,#2030,.F.);
#2658=ORIENTED_EDGE('',*,*,#2021,.T.);
#2659=ORIENTED_EDGE('',*,*,#2030,.T.);
#2660=ORIENTED_EDGE('',*,*,#2031,.F.);
#2661=ORIENTED_EDGE('',*,*,#2032,.F.);
#2662=ORIENTED_EDGE('',*,*,#2022,.T.);
#2663=ORIENTED_EDGE('',*,*,#2032,.T.);
#2664=ORIENTED_EDGE('',*,*,#2033,.F.);
#2665=ORIENTED_EDGE('',*,*,#2034,.F.);
#2666=ORIENTED_EDGE('',*,*,#2017,.T.);
#2667=ORIENTED_EDGE('',*,*,#2034,.T.);
#2668=ORIENTED_EDGE('',*,*,#2035,.F.);
#2669=ORIENTED_EDGE('',*,*,#2024,.F.);
#2670=ORIENTED_EDGE('',*,*,#2035,.T.);
#2671=ORIENTED_EDGE('',*,*,#2033,.T.);
#2672=ORIENTED_EDGE('',*,*,#2031,.T.);
#2673=ORIENTED_EDGE('',*,*,#2029,.T.);
#2674=ORIENTED_EDGE('',*,*,#2027,.T.);
#2675=ORIENTED_EDGE('',*,*,#2025,.T.);
#2676=ORIENTED_EDGE('',*,*,#2023,.F.);
#2677=ORIENTED_EDGE('',*,*,#2036,.T.);
#2678=ORIENTED_EDGE('',*,*,#2037,.T.);
#2679=ORIENTED_EDGE('',*,*,#2036,.F.);
#2680=ORIENTED_EDGE('',*,*,#2037,.F.);
#2681=ORIENTED_EDGE('',*,*,#2038,.F.);
#2682=ORIENTED_EDGE('',*,*,#2039,.F.);
#2683=ORIENTED_EDGE('',*,*,#2040,.F.);
#2684=ORIENTED_EDGE('',*,*,#2041,.T.);
#2685=ORIENTED_EDGE('',*,*,#2042,.F.);
#2686=ORIENTED_EDGE('',*,*,#2041,.F.);
#2687=ORIENTED_EDGE('',*,*,#2043,.F.);
#2688=ORIENTED_EDGE('',*,*,#2044,.T.);
#2689=ORIENTED_EDGE('',*,*,#2045,.F.);
#2690=ORIENTED_EDGE('',*,*,#2044,.F.);
#2691=ORIENTED_EDGE('',*,*,#2046,.F.);
#2692=ORIENTED_EDGE('',*,*,#2047,.T.);
#2693=ORIENTED_EDGE('',*,*,#2048,.F.);
#2694=ORIENTED_EDGE('',*,*,#2047,.F.);
#2695=ORIENTED_EDGE('',*,*,#2049,.F.);
#2696=ORIENTED_EDGE('',*,*,#2039,.T.);
#2697=ORIENTED_EDGE('',*,*,#2043,.T.);
#2698=ORIENTED_EDGE('',*,*,#2040,.T.);
#2699=ORIENTED_EDGE('',*,*,#2049,.T.);
#2700=ORIENTED_EDGE('',*,*,#2046,.T.);
#2701=ORIENTED_EDGE('',*,*,#2050,.T.);
#2702=ORIENTED_EDGE('',*,*,#2045,.T.);
#2703=ORIENTED_EDGE('',*,*,#2048,.T.);
#2704=ORIENTED_EDGE('',*,*,#2038,.T.);
#2705=ORIENTED_EDGE('',*,*,#2042,.T.);
#2706=ORIENTED_EDGE('',*,*,#2050,.F.);
#2707=ORIENTED_EDGE('',*,*,#2051,.T.);
#2708=ORIENTED_EDGE('',*,*,#2052,.T.);
#2709=ORIENTED_EDGE('',*,*,#2051,.F.);
#2710=ORIENTED_EDGE('',*,*,#2052,.F.);
#2711=ORIENTED_EDGE('',*,*,#2053,.F.);
#2712=ORIENTED_EDGE('',*,*,#2054,.T.);
#2713=ORIENTED_EDGE('',*,*,#2055,.F.);
#2714=ORIENTED_EDGE('',*,*,#2054,.F.);
#2715=ORIENTED_EDGE('',*,*,#2053,.T.);
#2716=ORIENTED_EDGE('',*,*,#2056,.F.);
#2717=ORIENTED_EDGE('',*,*,#2057,.F.);
#2718=ORIENTED_EDGE('',*,*,#2058,.T.);
#2719=ORIENTED_EDGE('',*,*,#2059,.F.);
#2720=ORIENTED_EDGE('',*,*,#2058,.F.);
#2721=ORIENTED_EDGE('',*,*,#2057,.T.);
#2722=ORIENTED_EDGE('',*,*,#2060,.F.);
#2723=ORIENTED_EDGE('',*,*,#2061,.F.);
#2724=ORIENTED_EDGE('',*,*,#2062,.T.);
#2725=ORIENTED_EDGE('',*,*,#2063,.F.);
#2726=ORIENTED_EDGE('',*,*,#2062,.F.);
#2727=ORIENTED_EDGE('',*,*,#2061,.T.);
#2728=ORIENTED_EDGE('',*,*,#2064,.F.);
#2729=ORIENTED_EDGE('',*,*,#2065,.F.);
#2730=ORIENTED_EDGE('',*,*,#2066,.T.);
#2731=ORIENTED_EDGE('',*,*,#2067,.F.);
#2732=ORIENTED_EDGE('',*,*,#2066,.F.);
#2733=ORIENTED_EDGE('',*,*,#2065,.T.);
#2734=ORIENTED_EDGE('',*,*,#2068,.F.);
#2735=ORIENTED_EDGE('',*,*,#2069,.F.);
#2736=ORIENTED_EDGE('',*,*,#2070,.T.);
#2737=ORIENTED_EDGE('',*,*,#2056,.T.);
#2738=ORIENTED_EDGE('',*,*,#2070,.F.);
#2739=ORIENTED_EDGE('',*,*,#2071,.F.);
#2740=ORIENTED_EDGE('',*,*,#2072,.T.);
#2741=ORIENTED_EDGE('',*,*,#2060,.T.);
#2742=ORIENTED_EDGE('',*,*,#2072,.F.);
#2743=ORIENTED_EDGE('',*,*,#2073,.F.);
#2744=ORIENTED_EDGE('',*,*,#2074,.T.);
#2745=ORIENTED_EDGE('',*,*,#2064,.T.);
#2746=ORIENTED_EDGE('',*,*,#2074,.F.);
#2747=ORIENTED_EDGE('',*,*,#2075,.F.);
#2748=ORIENTED_EDGE('',*,*,#2076,.T.);
#2749=ORIENTED_EDGE('',*,*,#2068,.T.);
#2750=ORIENTED_EDGE('',*,*,#2076,.F.);
#2751=ORIENTED_EDGE('',*,*,#2077,.F.);
#2752=ORIENTED_EDGE('',*,*,#2078,.T.);
#2753=ORIENTED_EDGE('',*,*,#2079,.F.);
#2754=ORIENTED_EDGE('',*,*,#2078,.F.);
#2755=ORIENTED_EDGE('',*,*,#2077,.T.);
#2756=ORIENTED_EDGE('',*,*,#2080,.F.);
#2757=ORIENTED_EDGE('',*,*,#2081,.F.);
#2758=ORIENTED_EDGE('',*,*,#2082,.T.);
#2759=ORIENTED_EDGE('',*,*,#2083,.F.);
#2760=ORIENTED_EDGE('',*,*,#2082,.F.);
#2761=ORIENTED_EDGE('',*,*,#2084,.F.);
#2762=ORIENTED_EDGE('',*,*,#2085,.T.);
#2763=ORIENTED_EDGE('',*,*,#2080,.T.);
#2764=ORIENTED_EDGE('',*,*,#2085,.F.);
#2765=ORIENTED_EDGE('',*,*,#2086,.F.);
#2766=ORIENTED_EDGE('',*,*,#2087,.T.);
#2767=ORIENTED_EDGE('',*,*,#2088,.F.);
#2768=ORIENTED_EDGE('',*,*,#2087,.F.);
#2769=ORIENTED_EDGE('',*,*,#2089,.T.);
#2770=ORIENTED_EDGE('',*,*,#2090,.T.);
#2771=ORIENTED_EDGE('',*,*,#2091,.F.);
#2772=ORIENTED_EDGE('',*,*,#2092,.F.);
#2773=ORIENTED_EDGE('',*,*,#2093,.T.);
#2774=ORIENTED_EDGE('',*,*,#2092,.T.);
#2775=ORIENTED_EDGE('',*,*,#2094,.F.);
#2776=ORIENTED_EDGE('',*,*,#2095,.F.);
#2777=ORIENTED_EDGE('',*,*,#2096,.T.);
#2778=ORIENTED_EDGE('',*,*,#2095,.T.);
#2779=ORIENTED_EDGE('',*,*,#2097,.F.);
#2780=ORIENTED_EDGE('',*,*,#2098,.F.);
#2781=ORIENTED_EDGE('',*,*,#2099,.T.);
#2782=ORIENTED_EDGE('',*,*,#2098,.T.);
#2783=ORIENTED_EDGE('',*,*,#2100,.F.);
#2784=ORIENTED_EDGE('',*,*,#2090,.F.);
#2785=ORIENTED_EDGE('',*,*,#2100,.T.);
#2786=ORIENTED_EDGE('',*,*,#2097,.T.);
#2787=ORIENTED_EDGE('',*,*,#2094,.T.);
#2788=ORIENTED_EDGE('',*,*,#2091,.T.);
#2789=ORIENTED_EDGE('',*,*,#2079,.T.);
#2790=ORIENTED_EDGE('',*,*,#2083,.T.);
#2791=ORIENTED_EDGE('',*,*,#2088,.T.);
#2792=ORIENTED_EDGE('',*,*,#2067,.T.);
#2793=ORIENTED_EDGE('',*,*,#2063,.T.);
#2794=ORIENTED_EDGE('',*,*,#2059,.T.);
#2795=ORIENTED_EDGE('',*,*,#2055,.T.);
#2796=ORIENTED_EDGE('',*,*,#2099,.F.);
#2797=ORIENTED_EDGE('',*,*,#2089,.F.);
#2798=ORIENTED_EDGE('',*,*,#2093,.F.);
#2799=ORIENTED_EDGE('',*,*,#2096,.F.);
#2800=ORIENTED_EDGE('',*,*,#2086,.T.);
#2801=ORIENTED_EDGE('',*,*,#2084,.T.);
#2802=ORIENTED_EDGE('',*,*,#2081,.T.);
#2803=ORIENTED_EDGE('',*,*,#2075,.T.);
#2804=ORIENTED_EDGE('',*,*,#2073,.T.);
#2805=ORIENTED_EDGE('',*,*,#2071,.T.);
#2806=ORIENTED_EDGE('',*,*,#2069,.T.);
#2807=ORIENTED_EDGE('',*,*,#2101,.F.);
#2808=ORIENTED_EDGE('',*,*,#2102,.T.);
#2809=ORIENTED_EDGE('',*,*,#2103,.F.);
#2810=ORIENTED_EDGE('',*,*,#2102,.F.);
#2811=ORIENTED_EDGE('',*,*,#2104,.F.);
#2812=ORIENTED_EDGE('',*,*,#2105,.T.);
#2813=ORIENTED_EDGE('',*,*,#2106,.F.);
#2814=ORIENTED_EDGE('',*,*,#2105,.F.);
#2815=ORIENTED_EDGE('',*,*,#2107,.F.);
#2816=ORIENTED_EDGE('',*,*,#2108,.T.);
#2817=ORIENTED_EDGE('',*,*,#2109,.F.);
#2818=ORIENTED_EDGE('',*,*,#2108,.F.);
#2819=ORIENTED_EDGE('',*,*,#2110,.F.);
#2820=ORIENTED_EDGE('',*,*,#2111,.T.);
#2821=ORIENTED_EDGE('',*,*,#2112,.F.);
#2822=ORIENTED_EDGE('',*,*,#2111,.F.);
#2823=ORIENTED_EDGE('',*,*,#2113,.F.);
#2824=ORIENTED_EDGE('',*,*,#2114,.T.);
#2825=ORIENTED_EDGE('',*,*,#2115,.F.);
#2826=ORIENTED_EDGE('',*,*,#2114,.F.);
#2827=ORIENTED_EDGE('',*,*,#2116,.F.);
#2828=ORIENTED_EDGE('',*,*,#2117,.T.);
#2829=ORIENTED_EDGE('',*,*,#2118,.F.);
#2830=ORIENTED_EDGE('',*,*,#2117,.F.);
#2831=ORIENTED_EDGE('',*,*,#2119,.F.);
#2832=ORIENTED_EDGE('',*,*,#2120,.T.);
#2833=ORIENTED_EDGE('',*,*,#2121,.F.);
#2834=ORIENTED_EDGE('',*,*,#2120,.F.);
#2835=ORIENTED_EDGE('',*,*,#2122,.T.);
#2836=ORIENTED_EDGE('',*,*,#2123,.T.);
#2837=ORIENTED_EDGE('',*,*,#2124,.F.);
#2838=ORIENTED_EDGE('',*,*,#2125,.F.);
#2839=ORIENTED_EDGE('',*,*,#2126,.T.);
#2840=ORIENTED_EDGE('',*,*,#2125,.T.);
#2841=ORIENTED_EDGE('',*,*,#2127,.F.);
#2842=ORIENTED_EDGE('',*,*,#2128,.F.);
#2843=ORIENTED_EDGE('',*,*,#2129,.T.);
#2844=ORIENTED_EDGE('',*,*,#2128,.T.);
#2845=ORIENTED_EDGE('',*,*,#2130,.F.);
#2846=ORIENTED_EDGE('',*,*,#2131,.F.);
#2847=ORIENTED_EDGE('',*,*,#2132,.T.);
#2848=ORIENTED_EDGE('',*,*,#2131,.T.);
#2849=ORIENTED_EDGE('',*,*,#2133,.F.);
#2850=ORIENTED_EDGE('',*,*,#2123,.F.);
#2851=ORIENTED_EDGE('',*,*,#2133,.T.);
#2852=ORIENTED_EDGE('',*,*,#2130,.T.);
#2853=ORIENTED_EDGE('',*,*,#2127,.T.);
#2854=ORIENTED_EDGE('',*,*,#2124,.T.);
#2855=ORIENTED_EDGE('',*,*,#2121,.T.);
#2856=ORIENTED_EDGE('',*,*,#2118,.T.);
#2857=ORIENTED_EDGE('',*,*,#2115,.T.);
#2858=ORIENTED_EDGE('',*,*,#2112,.T.);
#2859=ORIENTED_EDGE('',*,*,#2109,.T.);
#2860=ORIENTED_EDGE('',*,*,#2106,.T.);
#2861=ORIENTED_EDGE('',*,*,#2103,.T.);
#2862=ORIENTED_EDGE('',*,*,#2132,.F.);
#2863=ORIENTED_EDGE('',*,*,#2122,.F.);
#2864=ORIENTED_EDGE('',*,*,#2126,.F.);
#2865=ORIENTED_EDGE('',*,*,#2129,.F.);
#2866=ORIENTED_EDGE('',*,*,#2119,.T.);
#2867=ORIENTED_EDGE('',*,*,#2116,.T.);
#2868=ORIENTED_EDGE('',*,*,#2113,.T.);
#2869=ORIENTED_EDGE('',*,*,#2110,.T.);
#2870=ORIENTED_EDGE('',*,*,#2107,.T.);
#2871=ORIENTED_EDGE('',*,*,#2104,.T.);
#2872=ORIENTED_EDGE('',*,*,#2101,.T.);
#2873=ORIENTED_EDGE('',*,*,#2134,.F.);
#2874=ORIENTED_EDGE('',*,*,#2135,.T.);
#2875=ORIENTED_EDGE('',*,*,#2136,.F.);
#2876=ORIENTED_EDGE('',*,*,#2135,.F.);
#2877=ORIENTED_EDGE('',*,*,#2134,.T.);
#2878=ORIENTED_EDGE('',*,*,#2137,.F.);
#2879=ORIENTED_EDGE('',*,*,#2138,.F.);
#2880=ORIENTED_EDGE('',*,*,#2139,.F.);
#2881=ORIENTED_EDGE('',*,*,#2140,.F.);
#2882=ORIENTED_EDGE('',*,*,#2141,.F.);
#2883=ORIENTED_EDGE('',*,*,#2142,.F.);
#2884=ORIENTED_EDGE('',*,*,#2143,.F.);
#2885=ORIENTED_EDGE('',*,*,#2144,.T.);
#2886=ORIENTED_EDGE('',*,*,#2139,.T.);
#2887=ORIENTED_EDGE('',*,*,#2145,.T.);
#2888=ORIENTED_EDGE('',*,*,#2146,.F.);
#2889=ORIENTED_EDGE('',*,*,#2147,.F.);
#2890=ORIENTED_EDGE('',*,*,#2140,.T.);
#2891=ORIENTED_EDGE('',*,*,#2147,.T.);
#2892=ORIENTED_EDGE('',*,*,#2148,.F.);
#2893=ORIENTED_EDGE('',*,*,#2149,.F.);
#2894=ORIENTED_EDGE('',*,*,#2141,.T.);
#2895=ORIENTED_EDGE('',*,*,#2149,.T.);
#2896=ORIENTED_EDGE('',*,*,#2150,.F.);
#2897=ORIENTED_EDGE('',*,*,#2151,.F.);
#2898=ORIENTED_EDGE('',*,*,#2142,.T.);
#2899=ORIENTED_EDGE('',*,*,#2151,.T.);
#2900=ORIENTED_EDGE('',*,*,#2152,.F.);
#2901=ORIENTED_EDGE('',*,*,#2153,.F.);
#2902=ORIENTED_EDGE('',*,*,#2143,.T.);
#2903=ORIENTED_EDGE('',*,*,#2153,.T.);
#2904=ORIENTED_EDGE('',*,*,#2154,.F.);
#2905=ORIENTED_EDGE('',*,*,#2155,.F.);
#2906=ORIENTED_EDGE('',*,*,#2138,.T.);
#2907=ORIENTED_EDGE('',*,*,#2155,.T.);
#2908=ORIENTED_EDGE('',*,*,#2156,.F.);
#2909=ORIENTED_EDGE('',*,*,#2145,.F.);
#2910=ORIENTED_EDGE('',*,*,#2156,.T.);
#2911=ORIENTED_EDGE('',*,*,#2154,.T.);
#2912=ORIENTED_EDGE('',*,*,#2152,.T.);
#2913=ORIENTED_EDGE('',*,*,#2150,.T.);
#2914=ORIENTED_EDGE('',*,*,#2148,.T.);
#2915=ORIENTED_EDGE('',*,*,#2146,.T.);
#2916=ORIENTED_EDGE('',*,*,#2136,.T.);
#2917=ORIENTED_EDGE('',*,*,#2137,.T.);
#2918=ORIENTED_EDGE('',*,*,#2157,.T.);
#2919=ORIENTED_EDGE('',*,*,#2158,.T.);
#2920=ORIENTED_EDGE('',*,*,#2157,.F.);
#2921=ORIENTED_EDGE('',*,*,#2144,.F.);
#2922=ORIENTED_EDGE('',*,*,#2159,.T.);
#2923=ORIENTED_EDGE('',*,*,#2160,.T.);
#2924=ORIENTED_EDGE('',*,*,#2159,.F.);
#2925=ORIENTED_EDGE('',*,*,#2160,.F.);
#2926=ORIENTED_EDGE('',*,*,#2158,.F.);
#2927=ORIENTED_EDGE('',*,*,#2161,.F.);
#2928=ORIENTED_EDGE('',*,*,#2162,.T.);
#2929=ORIENTED_EDGE('',*,*,#2163,.F.);
#2930=ORIENTED_EDGE('',*,*,#2162,.F.);
#2931=ORIENTED_EDGE('',*,*,#2161,.T.);
#2932=ORIENTED_EDGE('',*,*,#2164,.F.);
#2933=ORIENTED_EDGE('',*,*,#2165,.T.);
#2934=ORIENTED_EDGE('',*,*,#2166,.T.);
#2935=ORIENTED_EDGE('',*,*,#2167,.T.);
#2936=ORIENTED_EDGE('',*,*,#2168,.T.);
#2937=ORIENTED_EDGE('',*,*,#2169,.T.);
#2938=ORIENTED_EDGE('',*,*,#2170,.T.);
#2939=ORIENTED_EDGE('',*,*,#2171,.T.);
#2940=ORIENTED_EDGE('',*,*,#2172,.F.);
#2941=ORIENTED_EDGE('',*,*,#2173,.F.);
#2942=ORIENTED_EDGE('',*,*,#2174,.F.);
#2943=ORIENTED_EDGE('',*,*,#2175,.F.);
#2944=ORIENTED_EDGE('',*,*,#2176,.F.);
#2945=ORIENTED_EDGE('',*,*,#2177,.F.);
#2946=ORIENTED_EDGE('',*,*,#2178,.F.);
#2947=ORIENTED_EDGE('',*,*,#2173,.T.);
#2948=ORIENTED_EDGE('',*,*,#2179,.T.);
#2949=ORIENTED_EDGE('',*,*,#2170,.F.);
#2950=ORIENTED_EDGE('',*,*,#2180,.F.);
#2951=ORIENTED_EDGE('',*,*,#2174,.T.);
#2952=ORIENTED_EDGE('',*,*,#2180,.T.);
#2953=ORIENTED_EDGE('',*,*,#2169,.F.);
#2954=ORIENTED_EDGE('',*,*,#2181,.F.);
#2955=ORIENTED_EDGE('',*,*,#2175,.T.);
#2956=ORIENTED_EDGE('',*,*,#2181,.T.);
#2957=ORIENTED_EDGE('',*,*,#2168,.F.);
#2958=ORIENTED_EDGE('',*,*,#2182,.F.);
#2959=ORIENTED_EDGE('',*,*,#2176,.T.);
#2960=ORIENTED_EDGE('',*,*,#2182,.T.);
#2961=ORIENTED_EDGE('',*,*,#2167,.F.);
#2962=ORIENTED_EDGE('',*,*,#2183,.F.);
#2963=ORIENTED_EDGE('',*,*,#2177,.T.);
#2964=ORIENTED_EDGE('',*,*,#2183,.T.);
#2965=ORIENTED_EDGE('',*,*,#2166,.F.);
#2966=ORIENTED_EDGE('',*,*,#2184,.F.);
#2967=ORIENTED_EDGE('',*,*,#2172,.T.);
#2968=ORIENTED_EDGE('',*,*,#2184,.T.);
#2969=ORIENTED_EDGE('',*,*,#2165,.F.);
#2970=ORIENTED_EDGE('',*,*,#2179,.F.);
#2971=ORIENTED_EDGE('',*,*,#2185,.F.);
#2972=ORIENTED_EDGE('',*,*,#2163,.T.);
#2973=ORIENTED_EDGE('',*,*,#2185,.T.);
#2974=ORIENTED_EDGE('',*,*,#2186,.T.);
#2975=ORIENTED_EDGE('',*,*,#2187,.F.);
#2976=ORIENTED_EDGE('',*,*,#2186,.F.);
#2977=ORIENTED_EDGE('',*,*,#2188,.F.);
#2978=ORIENTED_EDGE('',*,*,#2187,.T.);
#2979=ORIENTED_EDGE('',*,*,#2171,.F.);
#2980=ORIENTED_EDGE('',*,*,#2189,.T.);
#2981=ORIENTED_EDGE('',*,*,#2188,.T.);
#2982=ORIENTED_EDGE('',*,*,#2189,.F.);
#2983=ORIENTED_EDGE('',*,*,#2190,.F.);
#2984=ORIENTED_EDGE('',*,*,#2191,.T.);
#2985=ORIENTED_EDGE('',*,*,#2178,.T.);
#2986=ORIENTED_EDGE('',*,*,#2191,.F.);
#2987=ORIENTED_EDGE('',*,*,#2190,.T.);
#2988=ORIENTED_EDGE('',*,*,#2192,.F.);
#2989=ORIENTED_EDGE('',*,*,#2192,.T.);
#2990=ORIENTED_EDGE('',*,*,#2193,.T.);
#2991=ORIENTED_EDGE('',*,*,#2164,.T.);
#2992=ORIENTED_EDGE('',*,*,#2193,.F.);
#2993=ORIENTED_EDGE('',*,*,#2194,.F.);
#2994=ORIENTED_EDGE('',*,*,#2195,.T.);
#2995=ORIENTED_EDGE('',*,*,#2196,.F.);
#2996=ORIENTED_EDGE('',*,*,#2197,.T.);
#2997=ORIENTED_EDGE('',*,*,#2194,.T.);
#2998=ORIENTED_EDGE('',*,*,#2197,.F.);
#2999=ORIENTED_EDGE('',*,*,#2196,.T.);
#3000=ORIENTED_EDGE('',*,*,#2198,.F.);
#3001=ORIENTED_EDGE('',*,*,#2199,.F.);
#3002=ORIENTED_EDGE('',*,*,#2200,.T.);
#3003=ORIENTED_EDGE('',*,*,#2198,.T.);
#3004=ORIENTED_EDGE('',*,*,#2200,.F.);
#3005=ORIENTED_EDGE('',*,*,#2199,.T.);
#3006=ORIENTED_EDGE('',*,*,#2201,.F.);
#3007=ORIENTED_EDGE('',*,*,#2201,.T.);
#3008=ORIENTED_EDGE('',*,*,#2202,.T.);
#3009=ORIENTED_EDGE('',*,*,#2195,.F.);
#3010=ORIENTED_EDGE('',*,*,#2202,.F.);
#3011=ORIENTED_EDGE('',*,*,#2203,.F.);
#3012=ORIENTED_EDGE('',*,*,#2204,.F.);
#3013=ORIENTED_EDGE('',*,*,#2205,.T.);
#3014=ORIENTED_EDGE('',*,*,#2203,.T.);
#3015=ORIENTED_EDGE('',*,*,#2205,.F.);
#3016=ORIENTED_EDGE('',*,*,#2206,.F.);
#3017=ORIENTED_EDGE('',*,*,#2207,.T.);
#3018=ORIENTED_EDGE('',*,*,#2204,.T.);
#3019=ORIENTED_EDGE('',*,*,#2207,.F.);
#3020=ORIENTED_EDGE('',*,*,#2208,.F.);
#3021=ORIENTED_EDGE('',*,*,#2209,.T.);
#3022=ORIENTED_EDGE('',*,*,#2206,.T.);
#3023=ORIENTED_EDGE('',*,*,#2209,.F.);
#3024=ORIENTED_EDGE('',*,*,#2208,.T.);
#3025=ORIENTED_EDGE('',*,*,#2210,.F.);
#3026=ORIENTED_EDGE('',*,*,#2211,.F.);
#3027=ORIENTED_EDGE('',*,*,#2212,.T.);
#3028=ORIENTED_EDGE('',*,*,#2210,.T.);
#3029=ORIENTED_EDGE('',*,*,#2212,.F.);
#3030=ORIENTED_EDGE('',*,*,#2213,.F.);
#3031=ORIENTED_EDGE('',*,*,#2214,.T.);
#3032=ORIENTED_EDGE('',*,*,#2211,.T.);
#3033=ORIENTED_EDGE('',*,*,#2214,.F.);
#3034=ORIENTED_EDGE('',*,*,#2215,.F.);
#3035=ORIENTED_EDGE('',*,*,#2216,.T.);
#3036=ORIENTED_EDGE('',*,*,#2213,.T.);
#3037=ORIENTED_EDGE('',*,*,#2216,.F.);
#3038=ORIENTED_EDGE('',*,*,#2215,.T.);
#3039=ORIENTED_EDGE('',*,*,#2217,.T.);
#3040=ORIENTED_EDGE('',*,*,#2218,.T.);
#3041=ORIENTED_EDGE('',*,*,#2219,.T.);
#3042=ORIENTED_EDGE('',*,*,#2220,.F.);
#3043=ORIENTED_EDGE('',*,*,#2221,.T.);
#3044=ORIENTED_EDGE('',*,*,#2222,.T.);
#3045=ORIENTED_EDGE('',*,*,#2223,.T.);
#3046=ORIENTED_EDGE('',*,*,#2218,.F.);
#3047=ORIENTED_EDGE('',*,*,#2224,.T.);
#3048=ORIENTED_EDGE('',*,*,#2225,.T.);
#3049=ORIENTED_EDGE('',*,*,#2226,.T.);
#3050=ORIENTED_EDGE('',*,*,#2222,.F.);
#3051=ORIENTED_EDGE('',*,*,#2227,.T.);
#3052=ORIENTED_EDGE('',*,*,#2228,.T.);
#3053=ORIENTED_EDGE('',*,*,#2229,.T.);
#3054=ORIENTED_EDGE('',*,*,#2225,.F.);
#3055=ORIENTED_EDGE('',*,*,#2230,.T.);
#3056=ORIENTED_EDGE('',*,*,#2231,.T.);
#3057=ORIENTED_EDGE('',*,*,#2232,.T.);
#3058=ORIENTED_EDGE('',*,*,#2228,.F.);
#3059=ORIENTED_EDGE('',*,*,#2233,.T.);
#3060=ORIENTED_EDGE('',*,*,#2220,.T.);
#3061=ORIENTED_EDGE('',*,*,#2234,.T.);
#3062=ORIENTED_EDGE('',*,*,#2231,.F.);
#3063=ORIENTED_EDGE('',*,*,#2233,.F.);
#3064=ORIENTED_EDGE('',*,*,#2230,.F.);
#3065=ORIENTED_EDGE('',*,*,#2227,.F.);
#3066=ORIENTED_EDGE('',*,*,#2224,.F.);
#3067=ORIENTED_EDGE('',*,*,#2221,.F.);
#3068=ORIENTED_EDGE('',*,*,#2217,.F.);
#3069=ORIENTED_EDGE('',*,*,#2234,.F.);
#3070=ORIENTED_EDGE('',*,*,#2219,.F.);
#3071=ORIENTED_EDGE('',*,*,#2223,.F.);
#3072=ORIENTED_EDGE('',*,*,#2226,.F.);
#3073=ORIENTED_EDGE('',*,*,#2229,.F.);
#3074=ORIENTED_EDGE('',*,*,#2232,.F.);
#3075=CYLINDRICAL_SURFACE('',#3506,0.165);
#3076=CYLINDRICAL_SURFACE('',#3510,0.165);
#3077=CYLINDRICAL_SURFACE('',#3514,0.165);
#3078=CYLINDRICAL_SURFACE('',#3518,0.165);
#3079=CYLINDRICAL_SURFACE('',#3522,0.2);
#3080=CYLINDRICAL_SURFACE('',#3524,0.2);
#3081=CYLINDRICAL_SURFACE('',#3526,0.2);
#3082=CYLINDRICAL_SURFACE('',#3528,0.165);
#3083=CYLINDRICAL_SURFACE('',#3532,0.165);
#3084=CYLINDRICAL_SURFACE('',#3536,0.165);
#3085=CYLINDRICAL_SURFACE('',#3540,0.165);
#3086=CYLINDRICAL_SURFACE('',#3544,0.2);
#3087=CYLINDRICAL_SURFACE('',#3546,0.2);
#3088=CYLINDRICAL_SURFACE('',#3548,0.2);
#3089=CYLINDRICAL_SURFACE('',#3550,0.33);
#3090=CYLINDRICAL_SURFACE('',#3553,0.33);
#3091=CYLINDRICAL_SURFACE('',#3556,0.33);
#3092=CYLINDRICAL_SURFACE('',#3559,0.33);
#3093=CYLINDRICAL_SURFACE('',#3562,0.685);
#3094=CYLINDRICAL_SURFACE('',#3567,0.685);
#3095=CYLINDRICAL_SURFACE('',#3572,0.685);
#3096=CYLINDRICAL_SURFACE('',#3577,0.685);
#3097=CYLINDRICAL_SURFACE('',#3582,0.685);
#3098=CYLINDRICAL_SURFACE('',#3587,0.685);
#3099=CYLINDRICAL_SURFACE('',#3592,0.3);
#3100=CYLINDRICAL_SURFACE('',#3593,0.3);
#3101=CYLINDRICAL_SURFACE('',#3594,0.3);
#3102=CYLINDRICAL_SURFACE('',#3602,0.05);
#3103=CYLINDRICAL_SURFACE('',#3605,0.05);
#3104=CYLINDRICAL_SURFACE('',#3608,0.05);
#3105=CYLINDRICAL_SURFACE('',#3611,0.05);
#3106=CYLINDRICAL_SURFACE('',#3614,0.05);
#3107=CYLINDRICAL_SURFACE('',#3617,0.05);
#3108=CYLINDRICAL_SURFACE('',#3625,0.9);
#3109=CYLINDRICAL_SURFACE('',#3628,0.45);
#3110=CYLINDRICAL_SURFACE('',#3630,0.3);
#3111=CYLINDRICAL_SURFACE('',#3632,0.685);
#3112=CYLINDRICAL_SURFACE('',#3638,0.05);
#3113=CYLINDRICAL_SURFACE('',#3641,0.05);
#3114=CYLINDRICAL_SURFACE('',#3644,0.05);
#3115=CYLINDRICAL_SURFACE('',#3647,0.05);
#3116=CYLINDRICAL_SURFACE('',#3650,0.05);
#3117=CYLINDRICAL_SURFACE('',#3653,0.05);
#3118=CYLINDRICAL_SURFACE('',#3661,0.9);
#3119=CYLINDRICAL_SURFACE('',#3664,0.45);
#3120=CYLINDRICAL_SURFACE('',#3666,0.3);
#3121=CYLINDRICAL_SURFACE('',#3668,0.685);
#3122=CYLINDRICAL_SURFACE('',#3684,0.685);
#3123=CYLINDRICAL_SURFACE('',#3690,0.685);
#3124=CYLINDRICAL_SURFACE('',#3696,0.46);
#3125=CYLINDRICAL_SURFACE('',#3707,0.685);
#3126=CYLINDRICAL_SURFACE('',#3718,0.685);
#3127=CYLINDRICAL_SURFACE('',#3723,0.4);
#3128=CYLINDRICAL_SURFACE('',#3728,0.4);
#3129=CYLINDRICAL_SURFACE('',#3733,0.4);
#3130=CYLINDRICAL_SURFACE('',#3738,0.4);
#3131=CYLINDRICAL_SURFACE('',#3743,0.225);
#3132=CYLINDRICAL_SURFACE('',#3745,0.225);
#3133=CYLINDRICAL_SURFACE('',#3747,0.225);
#3134=CYLINDRICAL_SURFACE('',#3749,0.225);
#3135=CYLINDRICAL_SURFACE('',#3751,0.685);
#3136=CYLINDRICAL_SURFACE('',#3756,0.2);
#3137=CYLINDRICAL_SURFACE('',#3759,0.2);
#3138=CYLINDRICAL_SURFACE('',#3761,0.2);
#3139=CYLINDRICAL_SURFACE('',#3771,0.225);
#3140=CYLINDRICAL_SURFACE('',#3774,0.225);
#3141=CYLINDRICAL_SURFACE('',#3777,0.225);
#3142=CYLINDRICAL_SURFACE('',#3780,0.225);
#3143=CYLINDRICAL_SURFACE('',#3783,0.2);
#3144=CYLINDRICAL_SURFACE('',#3786,0.2);
#3145=CYLINDRICAL_SURFACE('',#3789,0.2);
#3146=CYLINDRICAL_SURFACE('',#3799,0.515);
#3147=CYLINDRICAL_SURFACE('',#3813,0.2);
#3148=CYLINDRICAL_SURFACE('',#3815,0.685);
#3149=CYLINDRICAL_SURFACE('',#3820,0.43);
#3150=CYLINDRICAL_SURFACE('',#3837,0.46);
#3151=CYLINDRICAL_SURFACE('',#3841,0.525);
#3152=CYLINDRICAL_SURFACE('',#3842,0.515);
#3153=CYLINDRICAL_SURFACE('',#3846,0.2);
#3154=CYLINDRICAL_SURFACE('',#3851,0.475);
#3155=CYLINDRICAL_SURFACE('',#3855,0.355);
#3156=CYLINDRICAL_SURFACE('',#3859,0.31);
#3157=CYLINDRICAL_SURFACE('',#3867,0.35);
#3158=CYLINDRICAL_SURFACE('',#3875,0.1954);
#3159=ADVANCED_FACE('',(#386),#3075,.F.);
#3160=ADVANCED_FACE('',(#387),#277,.T.);
#3161=ADVANCED_FACE('',(#388),#3076,.F.);
#3162=ADVANCED_FACE('',(#389),#278,.T.);
#3163=ADVANCED_FACE('',(#390),#3077,.F.);
#3164=ADVANCED_FACE('',(#391),#279,.T.);
#3165=ADVANCED_FACE('',(#392),#3078,.F.);
#3166=ADVANCED_FACE('',(#393),#280,.T.);
#3167=ADVANCED_FACE('',(#394),#3079,.F.);
#3168=ADVANCED_FACE('',(#395),#3080,.F.);
#3169=ADVANCED_FACE('',(#396),#3081,.F.);
#3170=ADVANCED_FACE('',(#397),#3082,.F.);
#3171=ADVANCED_FACE('',(#398),#281,.T.);
#3172=ADVANCED_FACE('',(#399),#3083,.F.);
#3173=ADVANCED_FACE('',(#400),#282,.T.);
#3174=ADVANCED_FACE('',(#401),#3084,.F.);
#3175=ADVANCED_FACE('',(#402),#283,.T.);
#3176=ADVANCED_FACE('',(#403),#3085,.F.);
#3177=ADVANCED_FACE('',(#404),#284,.T.);
#3178=ADVANCED_FACE('',(#405),#3086,.F.);
#3179=ADVANCED_FACE('',(#406),#3087,.F.);
#3180=ADVANCED_FACE('',(#407),#3088,.F.);
#3181=ADVANCED_FACE('',(#408),#3089,.F.);
#3182=ADVANCED_FACE('',(#409),#3090,.F.);
#3183=ADVANCED_FACE('',(#410),#3091,.F.);
#3184=ADVANCED_FACE('',(#411),#3092,.F.);
#3185=ADVANCED_FACE('',(#412),#3093,.F.);
#3186=ADVANCED_FACE('',(#413,#142),#285,.T.);
#3187=ADVANCED_FACE('',(#414),#3094,.F.);
#3188=ADVANCED_FACE('',(#415,#143),#286,.T.);
#3189=ADVANCED_FACE('',(#416),#3095,.F.);
#3190=ADVANCED_FACE('',(#417,#144),#287,.T.);
#3191=ADVANCED_FACE('',(#418),#3096,.F.);
#3192=ADVANCED_FACE('',(#419,#145),#288,.F.);
#3193=ADVANCED_FACE('',(#420),#3097,.F.);
#3194=ADVANCED_FACE('',(#421,#146),#289,.F.);
#3195=ADVANCED_FACE('',(#422),#3098,.F.);
#3196=ADVANCED_FACE('',(#423,#147),#290,.F.);
#3197=ADVANCED_FACE('',(#424),#3099,.F.);
#3198=ADVANCED_FACE('',(#425),#3100,.F.);
#3199=ADVANCED_FACE('',(#426),#3101,.F.);
#3200=ADVANCED_FACE('',(#427),#291,.T.);
#3201=ADVANCED_FACE('',(#428,#148,#149,#150),#292,.T.);
#3202=ADVANCED_FACE('',(#429),#293,.T.);
#3203=ADVANCED_FACE('',(#430,#151,#152,#153),#294,.T.);
#3204=ADVANCED_FACE('',(#431,#154,#155,#156,#157,#158,#159,#160,#161,#162,
#163,#164,#165,#166,#167,#168,#169,#170,#171),#295,.T.);
#3205=ADVANCED_FACE('',(#432,#172,#173,#174,#175),#296,.F.);
#3206=ADVANCED_FACE('',(#433),#3102,.F.);
#3207=ADVANCED_FACE('',(#434),#3103,.F.);
#3208=ADVANCED_FACE('',(#435),#3104,.F.);
#3209=ADVANCED_FACE('',(#436),#3105,.F.);
#3210=ADVANCED_FACE('',(#437),#3106,.F.);
#3211=ADVANCED_FACE('',(#438),#3107,.F.);
#3212=ADVANCED_FACE('',(#439,#176,#177,#178,#179,#180,#181),#297,.F.);
#3213=ADVANCED_FACE('',(#440,#182),#298,.F.);
#3214=ADVANCED_FACE('',(#441),#3108,.T.);
#3215=ADVANCED_FACE('',(#442,#183,#184,#185,#186,#187,#188),#299,.T.);
#3216=ADVANCED_FACE('',(#443),#3109,.T.);
#3217=ADVANCED_FACE('',(#444),#3110,.F.);
#3218=ADVANCED_FACE('',(#445),#3111,.T.);
#3219=ADVANCED_FACE('',(#446,#189),#300,.T.);
#3220=ADVANCED_FACE('',(#447,#190),#301,.F.);
#3221=ADVANCED_FACE('',(#448),#3112,.F.);
#3222=ADVANCED_FACE('',(#449),#3113,.F.);
#3223=ADVANCED_FACE('',(#450),#3114,.F.);
#3224=ADVANCED_FACE('',(#451),#3115,.F.);
#3225=ADVANCED_FACE('',(#452),#3116,.F.);
#3226=ADVANCED_FACE('',(#453),#3117,.F.);
#3227=ADVANCED_FACE('',(#454,#191,#192,#193,#194,#195,#196),#302,.F.);
#3228=ADVANCED_FACE('',(#455,#197),#303,.F.);
#3229=ADVANCED_FACE('',(#456),#3118,.T.);
#3230=ADVANCED_FACE('',(#457,#198,#199,#200,#201,#202,#203),#304,.T.);
#3231=ADVANCED_FACE('',(#458),#3119,.T.);
#3232=ADVANCED_FACE('',(#459),#3120,.F.);
#3233=ADVANCED_FACE('',(#460),#3121,.T.);
#3234=ADVANCED_FACE('',(#461,#204),#305,.T.);
#3235=ADVANCED_FACE('',(#462,#205),#306,.F.);
#3236=ADVANCED_FACE('',(#463,#206),#307,.F.);
#3237=ADVANCED_FACE('',(#464,#207),#308,.T.);
#3238=ADVANCED_FACE('',(#465),#309,.T.);
#3239=ADVANCED_FACE('',(#466),#310,.T.);
#3240=ADVANCED_FACE('',(#467),#311,.T.);
#3241=ADVANCED_FACE('',(#468),#312,.T.);
#3242=ADVANCED_FACE('',(#469),#313,.T.);
#3243=ADVANCED_FACE('',(#470),#314,.T.);
#3244=ADVANCED_FACE('',(#471),#3122,.T.);
#3245=ADVANCED_FACE('',(#472,#208),#315,.T.);
#3246=ADVANCED_FACE('',(#473),#89,.T.);
#3247=ADVANCED_FACE('',(#474),#3123,.T.);
#3248=ADVANCED_FACE('',(#475),#90,.T.);
#3249=ADVANCED_FACE('',(#476,#209),#316,.T.);
#3250=ADVANCED_FACE('',(#477),#3124,.F.);
#3251=ADVANCED_FACE('',(#478,#210),#317,.F.);
#3252=ADVANCED_FACE('',(#479),#318,.T.);
#3253=ADVANCED_FACE('',(#480),#319,.T.);
#3254=ADVANCED_FACE('',(#481),#320,.T.);
#3255=ADVANCED_FACE('',(#482),#321,.T.);
#3256=ADVANCED_FACE('',(#483),#322,.T.);
#3257=ADVANCED_FACE('',(#484),#323,.T.);
#3258=ADVANCED_FACE('',(#485),#324,.T.);
#3259=ADVANCED_FACE('',(#486),#3125,.T.);
#3260=ADVANCED_FACE('',(#487),#325,.F.);
#3261=ADVANCED_FACE('',(#488),#326,.F.);
#3262=ADVANCED_FACE('',(#489),#327,.F.);
#3263=ADVANCED_FACE('',(#490),#328,.F.);
#3264=ADVANCED_FACE('',(#491),#329,.F.);
#3265=ADVANCED_FACE('',(#492),#330,.T.);
#3266=ADVANCED_FACE('',(#493,#211),#331,.T.);
#3267=ADVANCED_FACE('',(#494),#3126,.T.);
#3268=ADVANCED_FACE('',(#495),#332,.F.);
#3269=ADVANCED_FACE('',(#496),#3127,.F.);
#3270=ADVANCED_FACE('',(#497,#212),#333,.T.);
#3271=ADVANCED_FACE('',(#498),#3128,.F.);
#3272=ADVANCED_FACE('',(#499,#213),#334,.T.);
#3273=ADVANCED_FACE('',(#500),#3129,.F.);
#3274=ADVANCED_FACE('',(#501,#214),#335,.T.);
#3275=ADVANCED_FACE('',(#502),#3130,.F.);
#3276=ADVANCED_FACE('',(#503,#215),#336,.T.);
#3277=ADVANCED_FACE('',(#504),#3131,.F.);
#3278=ADVANCED_FACE('',(#505),#3132,.F.);
#3279=ADVANCED_FACE('',(#506),#3133,.F.);
#3280=ADVANCED_FACE('',(#507),#3134,.F.);
#3281=ADVANCED_FACE('',(#508),#3135,.F.);
#3282=ADVANCED_FACE('',(#509,#216),#337,.T.);
#3283=ADVANCED_FACE('',(#510),#3136,.F.);
#3284=ADVANCED_FACE('',(#511),#3137,.F.);
#3285=ADVANCED_FACE('',(#512),#3138,.F.);
#3286=ADVANCED_FACE('',(#513),#338,.T.);
#3287=ADVANCED_FACE('',(#514),#339,.T.);
#3288=ADVANCED_FACE('',(#515),#340,.T.);
#3289=ADVANCED_FACE('',(#516),#341,.T.);
#3290=ADVANCED_FACE('',(#517,#217,#218,#219,#220,#221,#222,#223),#342,.T.);
#3291=ADVANCED_FACE('',(#518,#224,#225,#226,#227,#228,#229,#230),#343,.F.);
#3292=ADVANCED_FACE('',(#519),#3139,.F.);
#3293=ADVANCED_FACE('',(#520),#3140,.F.);
#3294=ADVANCED_FACE('',(#521),#3141,.F.);
#3295=ADVANCED_FACE('',(#522),#3142,.F.);
#3296=ADVANCED_FACE('',(#523),#3143,.F.);
#3297=ADVANCED_FACE('',(#524),#3144,.F.);
#3298=ADVANCED_FACE('',(#525),#3145,.F.);
#3299=ADVANCED_FACE('',(#526),#344,.T.);
#3300=ADVANCED_FACE('',(#527),#345,.T.);
#3301=ADVANCED_FACE('',(#528),#346,.T.);
#3302=ADVANCED_FACE('',(#529),#347,.T.);
#3303=ADVANCED_FACE('',(#530,#231,#232,#233,#234,#235,#236,#237),#348,.T.);
#3304=ADVANCED_FACE('',(#531,#238,#239,#240,#241,#242,#243,#244),#349,.F.);
#3305=ADVANCED_FACE('',(#532),#3146,.F.);
#3306=ADVANCED_FACE('',(#533,#245),#350,.T.);
#3307=ADVANCED_FACE('',(#534,#246),#351,.F.);
#3308=ADVANCED_FACE('',(#535),#352,.T.);
#3309=ADVANCED_FACE('',(#536),#353,.T.);
#3310=ADVANCED_FACE('',(#537),#354,.T.);
#3311=ADVANCED_FACE('',(#538),#355,.T.);
#3312=ADVANCED_FACE('',(#539),#356,.T.);
#3313=ADVANCED_FACE('',(#540),#357,.T.);
#3314=ADVANCED_FACE('',(#541,#247),#358,.T.);
#3315=ADVANCED_FACE('',(#542),#3147,.F.);
#3316=ADVANCED_FACE('',(#543),#3148,.T.);
#3317=ADVANCED_FACE('',(#544,#248),#359,.F.);
#3318=ADVANCED_FACE('',(#545),#3149,.F.);
#3319=ADVANCED_FACE('',(#546,#249),#360,.T.);
#3320=ADVANCED_FACE('',(#547,#250),#361,.T.);
#3321=ADVANCED_FACE('',(#548,#251),#362,.F.);
#3322=ADVANCED_FACE('',(#549),#363,.T.);
#3323=ADVANCED_FACE('',(#550),#364,.T.);
#3324=ADVANCED_FACE('',(#551),#365,.T.);
#3325=ADVANCED_FACE('',(#552),#366,.T.);
#3326=ADVANCED_FACE('',(#553),#367,.T.);
#3327=ADVANCED_FACE('',(#554),#368,.T.);
#3328=ADVANCED_FACE('',(#555,#252),#369,.T.);
#3329=ADVANCED_FACE('',(#556),#3150,.F.);
#3330=ADVANCED_FACE('',(#557,#253),#370,.T.);
#3331=ADVANCED_FACE('',(#558),#3151,.T.);
#3332=ADVANCED_FACE('',(#559),#3152,.T.);
#3333=ADVANCED_FACE('',(#560,#254),#371,.T.);
#3334=ADVANCED_FACE('',(#561),#3153,.F.);
#3335=ADVANCED_FACE('',(#562,#255),#372,.T.);
#3336=ADVANCED_FACE('',(#563),#3154,.T.);
#3337=ADVANCED_FACE('',(#564,#256),#373,.T.);
#3338=ADVANCED_FACE('',(#565),#3155,.T.);
#3339=ADVANCED_FACE('',(#566,#257),#374,.T.);
#3340=ADVANCED_FACE('',(#567),#3156,.F.);
#3341=ADVANCED_FACE('',(#568),#375,.T.);
#3342=ADVANCED_FACE('',(#569),#91,.T.);
#3343=ADVANCED_FACE('',(#570),#3157,.T.);
#3344=ADVANCED_FACE('',(#571),#92,.T.);
#3345=ADVANCED_FACE('',(#572,#258),#376,.T.);
#3346=ADVANCED_FACE('',(#573),#93,.T.);
#3347=ADVANCED_FACE('',(#574),#3158,.T.);
#3348=ADVANCED_FACE('',(#575),#94,.T.);
#3349=ADVANCED_FACE('',(#576),#377,.T.);
#3350=ADVANCED_FACE('',(#577),#378,.F.);
#3351=ADVANCED_FACE('',(#578),#379,.F.);
#3352=ADVANCED_FACE('',(#579),#380,.F.);
#3353=ADVANCED_FACE('',(#580),#381,.F.);
#3354=ADVANCED_FACE('',(#581),#382,.F.);
#3355=ADVANCED_FACE('',(#582),#383,.F.);
#3356=ADVANCED_FACE('',(#583),#384,.F.);
#3357=ADVANCED_FACE('',(#584),#385,.F.);
#3358=CLOSED_SHELL('',(#3159,#3160,#3161,#3162,#3163,#3164,#3165,#3166,
#3167,#3168,#3169,#3170,#3171,#3172,#3173,#3174,#3175,#3176,#3177,#3178,
#3179,#3180,#3181,#3182,#3183,#3184,#3185,#3186,#3187,#3188,#3189,#3190,
#3191,#3192,#3193,#3194,#3195,#3196,#3197,#3198,#3199,#3200,#3201,#3202,
#3203,#3204,#3205));
#3359=CLOSED_SHELL('',(#3206,#3207,#3208,#3209,#3210,#3211,#3212,#3213,
#3214,#3215,#3216,#3217,#3218,#3219,#3220));
#3360=CLOSED_SHELL('',(#3221,#3222,#3223,#3224,#3225,#3226,#3227,#3228,
#3229,#3230,#3231,#3232,#3233,#3234,#3235));
#3361=CLOSED_SHELL('',(#3236,#3237,#3238,#3239,#3240,#3241,#3242,#3243,
#3244,#3245,#3246,#3247,#3248,#3249,#3250));
#3362=CLOSED_SHELL('',(#3251,#3252,#3253,#3254,#3255,#3256,#3257,#3258,
#3259,#3260));
#3363=CLOSED_SHELL('',(#3261,#3262,#3263,#3264,#3265,#3266,#3267,#3268));
#3364=CLOSED_SHELL('',(#3269,#3270,#3271,#3272,#3273,#3274,#3275,#3276,
#3277,#3278,#3279,#3280,#3281,#3282,#3283,#3284,#3285,#3286,#3287,#3288,
#3289,#3290,#3291));
#3365=CLOSED_SHELL('',(#3292,#3293,#3294,#3295,#3296,#3297,#3298,#3299,
#3300,#3301,#3302,#3303,#3304));
#3366=CLOSED_SHELL('',(#3305,#3306,#3307,#3308,#3309,#3310,#3311,#3312,
#3313,#3314,#3315,#3316,#3317));
#3367=CLOSED_SHELL('',(#3318,#3319,#3320,#3321,#3322,#3323,#3324,#3325,
#3326,#3327,#3328,#3329,#3330,#3331,#3332,#3333,#3334));
#3368=CLOSED_SHELL('',(#3335,#3336,#3337,#3338,#3339,#3340));
#3369=CLOSED_SHELL('',(#3341,#3342,#3343,#3344,#3345,#3346,#3347,#3348,
#3349));
#3370=CLOSED_SHELL('',(#3350,#3351,#3352,#3353,#3354,#3355,#3356,#3357));
#3371=DERIVED_UNIT_ELEMENT(#3395,1.);
#3372=DERIVED_UNIT_ELEMENT(#6115,-3.);
#3373=DERIVED_UNIT_ELEMENT(#3395,1.);
#3374=DERIVED_UNIT_ELEMENT(#6115,-3.);
#3375=DERIVED_UNIT_ELEMENT(#3395,1.);
#3376=DERIVED_UNIT_ELEMENT(#6115,-3.);
#3377=DERIVED_UNIT_ELEMENT(#3395,1.);
#3378=DERIVED_UNIT_ELEMENT(#6115,-3.);
#3379=DERIVED_UNIT_ELEMENT(#3395,1.);
#3380=DERIVED_UNIT_ELEMENT(#6115,-3.);
#3381=DERIVED_UNIT_ELEMENT(#3395,1.);
#3382=DERIVED_UNIT_ELEMENT(#6115,-3.);
#3383=DERIVED_UNIT_ELEMENT(#3395,1.);
#3384=DERIVED_UNIT_ELEMENT(#6115,-3.);
#3385=DERIVED_UNIT_ELEMENT(#3395,1.);
#3386=DERIVED_UNIT_ELEMENT(#6115,-3.);
#3387=DERIVED_UNIT_ELEMENT(#3395,1.);
#3388=DERIVED_UNIT_ELEMENT(#6115,-3.);
#3389=DERIVED_UNIT_ELEMENT(#3395,1.);
#3390=DERIVED_UNIT_ELEMENT(#6115,-3.);
#3391=DERIVED_UNIT_ELEMENT(#3395,1.);
#3392=DERIVED_UNIT_ELEMENT(#6115,-3.);
#3393=DERIVED_UNIT_ELEMENT(#3395,1.);
#3394=DERIVED_UNIT_ELEMENT(#6115,-3.);
#3395=(
MASS_UNIT()
NAMED_UNIT(*)
SI_UNIT(.KILO.,.GRAM.)
);
#3396=DERIVED_UNIT((#3371,#3372));
#3397=DERIVED_UNIT((#3373,#3374));
#3398=DERIVED_UNIT((#3375,#3376));
#3399=DERIVED_UNIT((#3377,#3378));
#3400=DERIVED_UNIT((#3379,#3380));
#3401=DERIVED_UNIT((#3381,#3382));
#3402=DERIVED_UNIT((#3383,#3384));
#3403=DERIVED_UNIT((#3385,#3386));
#3404=DERIVED_UNIT((#3387,#3388));
#3405=DERIVED_UNIT((#3389,#3390));
#3406=DERIVED_UNIT((#3391,#3392));
#3407=DERIVED_UNIT((#3393,#3394));
#3408=MEASURE_REPRESENTATION_ITEM('density measure',
POSITIVE_RATIO_MEASURE(7850.),#3396);
#3409=MEASURE_REPRESENTATION_ITEM('density measure',
POSITIVE_RATIO_MEASURE(7850.),#3397);
#3410=MEASURE_REPRESENTATION_ITEM('density measure',
POSITIVE_RATIO_MEASURE(7850.),#3398);
#3411=MEASURE_REPRESENTATION_ITEM('density measure',
POSITIVE_RATIO_MEASURE(7850.),#3399);
#3412=MEASURE_REPRESENTATION_ITEM('density measure',
POSITIVE_RATIO_MEASURE(7850.),#3400);
#3413=MEASURE_REPRESENTATION_ITEM('density measure',
POSITIVE_RATIO_MEASURE(7850.),#3401);
#3414=MEASURE_REPRESENTATION_ITEM('density measure',
POSITIVE_RATIO_MEASURE(7850.),#3402);
#3415=MEASURE_REPRESENTATION_ITEM('density measure',
POSITIVE_RATIO_MEASURE(7850.),#3403);
#3416=MEASURE_REPRESENTATION_ITEM('density measure',
POSITIVE_RATIO_MEASURE(7850.),#3404);
#3417=MEASURE_REPRESENTATION_ITEM('density measure',
POSITIVE_RATIO_MEASURE(7850.),#3405);
#3418=MEASURE_REPRESENTATION_ITEM('density measure',
POSITIVE_RATIO_MEASURE(7850.),#3406);
#3419=MEASURE_REPRESENTATION_ITEM('density measure',
POSITIVE_RATIO_MEASURE(7850.),#3407);
#3420=PROPERTY_DEFINITION_REPRESENTATION(#3480,#3444);
#3421=PROPERTY_DEFINITION_REPRESENTATION(#3481,#3445);
#3422=PROPERTY_DEFINITION_REPRESENTATION(#3482,#3446);
#3423=PROPERTY_DEFINITION_REPRESENTATION(#3483,#3447);
#3424=PROPERTY_DEFINITION_REPRESENTATION(#3484,#3448);
#3425=PROPERTY_DEFINITION_REPRESENTATION(#3485,#3449);
#3426=PROPERTY_DEFINITION_REPRESENTATION(#3486,#3450);
#3427=PROPERTY_DEFINITION_REPRESENTATION(#3487,#3451);
#3428=PROPERTY_DEFINITION_REPRESENTATION(#3488,#3452);
#3429=PROPERTY_DEFINITION_REPRESENTATION(#3489,#3453);
#3430=PROPERTY_DEFINITION_REPRESENTATION(#3490,#3454);
#3431=PROPERTY_DEFINITION_REPRESENTATION(#3491,#3455);
#3432=PROPERTY_DEFINITION_REPRESENTATION(#3492,#3456);
#3433=PROPERTY_DEFINITION_REPRESENTATION(#3493,#3457);
#3434=PROPERTY_DEFINITION_REPRESENTATION(#3494,#3458);
#3435=PROPERTY_DEFINITION_REPRESENTATION(#3495,#3459);
#3436=PROPERTY_DEFINITION_REPRESENTATION(#3496,#3460);
#3437=PROPERTY_DEFINITION_REPRESENTATION(#3497,#3461);
#3438=PROPERTY_DEFINITION_REPRESENTATION(#3498,#3462);
#3439=PROPERTY_DEFINITION_REPRESENTATION(#3499,#3463);
#3440=PROPERTY_DEFINITION_REPRESENTATION(#3500,#3464);
#3441=PROPERTY_DEFINITION_REPRESENTATION(#3501,#3465);
#3442=PROPERTY_DEFINITION_REPRESENTATION(#3502,#3466);
#3443=PROPERTY_DEFINITION_REPRESENTATION(#3503,#3467);
#3444=REPRESENTATION('material name',(#3468),#6099);
#3445=REPRESENTATION('density',(#3408),#6099);
#3446=REPRESENTATION('material name',(#3469),#6100);
#3447=REPRESENTATION('density',(#3409),#6100);
#3448=REPRESENTATION('material name',(#3470),#6101);
#3449=REPRESENTATION('density',(#3410),#6101);
#3450=REPRESENTATION('material name',(#3471),#6102);
#3451=REPRESENTATION('density',(#3411),#6102);
#3452=REPRESENTATION('material name',(#3472),#6103);
#3453=REPRESENTATION('density',(#3412),#6103);
#3454=REPRESENTATION('material name',(#3473),#6104);
#3455=REPRESENTATION('density',(#3413),#6104);
#3456=REPRESENTATION('material name',(#3474),#6106);
#3457=REPRESENTATION('density',(#3414),#6106);
#3458=REPRESENTATION('material name',(#3475),#6107);
#3459=REPRESENTATION('density',(#3415),#6107);
#3460=REPRESENTATION('material name',(#3476),#6108);
#3461=REPRESENTATION('density',(#3416),#6108);
#3462=REPRESENTATION('material name',(#3477),#6110);
#3463=REPRESENTATION('density',(#3417),#6110);
#3464=REPRESENTATION('material name',(#3478),#6111);
#3465=REPRESENTATION('density',(#3418),#6111);
#3466=REPRESENTATION('material name',(#3479),#6112);
#3467=REPRESENTATION('density',(#3419),#6112);
#3468=DESCRIPTIVE_REPRESENTATION_ITEM('Steel','Steel');
#3469=DESCRIPTIVE_REPRESENTATION_ITEM('Steel','Steel');
#3470=DESCRIPTIVE_REPRESENTATION_ITEM('Steel','Steel');
#3471=DESCRIPTIVE_REPRESENTATION_ITEM('Steel','Steel');
#3472=DESCRIPTIVE_REPRESENTATION_ITEM('Steel','Steel');
#3473=DESCRIPTIVE_REPRESENTATION_ITEM('Steel','Steel');
#3474=DESCRIPTIVE_REPRESENTATION_ITEM('Steel','Steel');
#3475=DESCRIPTIVE_REPRESENTATION_ITEM('Steel','Steel');
#3476=DESCRIPTIVE_REPRESENTATION_ITEM('Steel','Steel');
#3477=DESCRIPTIVE_REPRESENTATION_ITEM('Steel','Steel');
#3478=DESCRIPTIVE_REPRESENTATION_ITEM('Steel','Steel');
#3479=DESCRIPTIVE_REPRESENTATION_ITEM('Steel','Steel');
#3480=PROPERTY_DEFINITION('material property','material name',#6184);
#3481=PROPERTY_DEFINITION('material property','density of part',#6184);
#3482=PROPERTY_DEFINITION('material property','material name',#6185);
#3483=PROPERTY_DEFINITION('material property','density of part',#6185);
#3484=PROPERTY_DEFINITION('material property','material name',#6186);
#3485=PROPERTY_DEFINITION('material property','density of part',#6186);
#3486=PROPERTY_DEFINITION('material property','material name',#6187);
#3487=PROPERTY_DEFINITION('material property','density of part',#6187);
#3488=PROPERTY_DEFINITION('material property','material name',#6188);
#3489=PROPERTY_DEFINITION('material property','density of part',#6188);
#3490=PROPERTY_DEFINITION('material property','material name',#6189);
#3491=PROPERTY_DEFINITION('material property','density of part',#6189);
#3492=PROPERTY_DEFINITION('material property','material name',#6191);
#3493=PROPERTY_DEFINITION('material property','density of part',#6191);
#3494=PROPERTY_DEFINITION('material property','material name',#6192);
#3495=PROPERTY_DEFINITION('material property','density of part',#6192);
#3496=PROPERTY_DEFINITION('material property','material name',#6193);
#3497=PROPERTY_DEFINITION('material property','density of part',#6193);
#3498=PROPERTY_DEFINITION('material property','material name',#6195);
#3499=PROPERTY_DEFINITION('material property','density of part',#6195);
#3500=PROPERTY_DEFINITION('material property','material name',#6196);
#3501=PROPERTY_DEFINITION('material property','density of part',#6196);
#3502=PROPERTY_DEFINITION('material property','material name',#6197);
#3503=PROPERTY_DEFINITION('material property','density of part',#6197);
#3504=AXIS2_PLACEMENT_3D('',#4941,#3905,#3906);
#3505=AXIS2_PLACEMENT_3D('',#4942,#3907,#3908);
#3506=AXIS2_PLACEMENT_3D('',#4943,#3909,#3910);
#3507=AXIS2_PLACEMENT_3D('',#4945,#3911,#3912);
#3508=AXIS2_PLACEMENT_3D('',#4948,#3914,#3915);
#3509=AXIS2_PLACEMENT_3D('',#4949,#3916,#3917);
#3510=AXIS2_PLACEMENT_3D('',#4950,#3918,#3919);
#3511=AXIS2_PLACEMENT_3D('',#4952,#3920,#3921);
#3512=AXIS2_PLACEMENT_3D('',#4955,#3923,#3924);
#3513=AXIS2_PLACEMENT_3D('',#4956,#3925,#3926);
#3514=AXIS2_PLACEMENT_3D('',#4957,#3927,#3928);
#3515=AXIS2_PLACEMENT_3D('',#4959,#3929,#3930);
#3516=AXIS2_PLACEMENT_3D('',#4962,#3932,#3933);
#3517=AXIS2_PLACEMENT_3D('',#4963,#3934,#3935);
#3518=AXIS2_PLACEMENT_3D('',#4964,#3936,#3937);
#3519=AXIS2_PLACEMENT_3D('',#4966,#3938,#3939);
#3520=AXIS2_PLACEMENT_3D('',#4969,#3941,#3942);
#3521=AXIS2_PLACEMENT_3D('',#4970,#3943,#3944);
#3522=AXIS2_PLACEMENT_3D('',#4971,#3945,#3946);
#3523=AXIS2_PLACEMENT_3D('',#4997,#3948,#3949);
#3524=AXIS2_PLACEMENT_3D('',#5016,#3950,#3951);
#3525=AXIS2_PLACEMENT_3D('',#5042,#3953,#3954);
#3526=AXIS2_PLACEMENT_3D('',#5061,#3955,#3956);
#3527=AXIS2_PLACEMENT_3D('',#5087,#3958,#3959);
#3528=AXIS2_PLACEMENT_3D('',#5106,#3960,#3961);
#3529=AXIS2_PLACEMENT_3D('',#5108,#3962,#3963);
#3530=AXIS2_PLACEMENT_3D('',#5111,#3965,#3966);
#3531=AXIS2_PLACEMENT_3D('',#5112,#3967,#3968);
#3532=AXIS2_PLACEMENT_3D('',#5113,#3969,#3970);
#3533=AXIS2_PLACEMENT_3D('',#5115,#3971,#3972);
#3534=AXIS2_PLACEMENT_3D('',#5118,#3974,#3975);
#3535=AXIS2_PLACEMENT_3D('',#5119,#3976,#3977);
#3536=AXIS2_PLACEMENT_3D('',#5120,#3978,#3979);
#3537=AXIS2_PLACEMENT_3D('',#5122,#3980,#3981);
#3538=AXIS2_PLACEMENT_3D('',#5125,#3983,#3984);
#3539=AXIS2_PLACEMENT_3D('',#5126,#3985,#3986);
#3540=AXIS2_PLACEMENT_3D('',#5127,#3987,#3988);
#3541=AXIS2_PLACEMENT_3D('',#5129,#3989,#3990);
#3542=AXIS2_PLACEMENT_3D('',#5132,#3992,#3993);
#3543=AXIS2_PLACEMENT_3D('',#5133,#3994,#3995);
#3544=AXIS2_PLACEMENT_3D('',#5134,#3996,#3997);
#3545=AXIS2_PLACEMENT_3D('',#5160,#3999,#4000);
#3546=AXIS2_PLACEMENT_3D('',#5179,#4001,#4002);
#3547=AXIS2_PLACEMENT_3D('',#5205,#4004,#4005);
#3548=AXIS2_PLACEMENT_3D('',#5224,#4006,#4007);
#3549=AXIS2_PLACEMENT_3D('',#5250,#4009,#4010);
#3550=AXIS2_PLACEMENT_3D('',#5269,#4011,#4012);
#3551=AXIS2_PLACEMENT_3D('',#5271,#4013,#4014);
#3552=AXIS2_PLACEMENT_3D('',#5274,#4016,#4017);
#3553=AXIS2_PLACEMENT_3D('',#5275,#4018,#4019);
#3554=AXIS2_PLACEMENT_3D('',#5277,#4020,#4021);
#3555=AXIS2_PLACEMENT_3D('',#5280,#4023,#4024);
#3556=AXIS2_PLACEMENT_3D('',#5281,#4025,#4026);
#3557=AXIS2_PLACEMENT_3D('',#5283,#4027,#4028);
#3558=AXIS2_PLACEMENT_3D('',#5286,#4030,#4031);
#3559=AXIS2_PLACEMENT_3D('',#5287,#4032,#4033);
#3560=AXIS2_PLACEMENT_3D('',#5289,#4034,#4035);
#3561=AXIS2_PLACEMENT_3D('',#5292,#4037,#4038);
#3562=AXIS2_PLACEMENT_3D('',#5293,#4039,#4040);
#3563=AXIS2_PLACEMENT_3D('',#5295,#4041,#4042);
#3564=AXIS2_PLACEMENT_3D('',#5298,#4044,#4045);
#3565=AXIS2_PLACEMENT_3D('',#5299,#4046,#4047);
#3566=AXIS2_PLACEMENT_3D('',#5301,#4048,#4049);
#3567=AXIS2_PLACEMENT_3D('',#5302,#4050,#4051);
#3568=AXIS2_PLACEMENT_3D('',#5304,#4052,#4053);
#3569=AXIS2_PLACEMENT_3D('',#5307,#4055,#4056);
#3570=AXIS2_PLACEMENT_3D('',#5308,#4057,#4058);
#3571=AXIS2_PLACEMENT_3D('',#5310,#4059,#4060);
#3572=AXIS2_PLACEMENT_3D('',#5311,#4061,#4062);
#3573=AXIS2_PLACEMENT_3D('',#5313,#4063,#4064);
#3574=AXIS2_PLACEMENT_3D('',#5316,#4066,#4067);
#3575=AXIS2_PLACEMENT_3D('',#5317,#4068,#4069);
#3576=AXIS2_PLACEMENT_3D('',#5319,#4070,#4071);
#3577=AXIS2_PLACEMENT_3D('',#5320,#4072,#4073);
#3578=AXIS2_PLACEMENT_3D('',#5322,#4074,#4075);
#3579=AXIS2_PLACEMENT_3D('',#5325,#4077,#4078);
#3580=AXIS2_PLACEMENT_3D('',#5326,#4079,#4080);
#3581=AXIS2_PLACEMENT_3D('',#5328,#4081,#4082);
#3582=AXIS2_PLACEMENT_3D('',#5329,#4083,#4084);
#3583=AXIS2_PLACEMENT_3D('',#5331,#4085,#4086);
#3584=AXIS2_PLACEMENT_3D('',#5334,#4088,#4089);
#3585=AXIS2_PLACEMENT_3D('',#5335,#4090,#4091);
#3586=AXIS2_PLACEMENT_3D('',#5337,#4092,#4093);
#3587=AXIS2_PLACEMENT_3D('',#5338,#4094,#4095);
#3588=AXIS2_PLACEMENT_3D('',#5340,#4096,#4097);
#3589=AXIS2_PLACEMENT_3D('',#5343,#4099,#4100);
#3590=AXIS2_PLACEMENT_3D('',#5344,#4101,#4102);
#3591=AXIS2_PLACEMENT_3D('',#5346,#4103,#4104);
#3592=AXIS2_PLACEMENT_3D('',#5347,#4105,#4106);
#3593=AXIS2_PLACEMENT_3D('',#5351,#4110,#4111);
#3594=AXIS2_PLACEMENT_3D('',#5355,#4115,#4116);
#3595=AXIS2_PLACEMENT_3D('',#5359,#4120,#4121);
#3596=AXIS2_PLACEMENT_3D('',#5368,#4126,#4127);
#3597=AXIS2_PLACEMENT_3D('',#5374,#4131,#4132);
#3598=AXIS2_PLACEMENT_3D('',#5380,#4136,#4137);
#3599=AXIS2_PLACEMENT_3D('',#5383,#4140,#4141);
#3600=AXIS2_PLACEMENT_3D('',#5384,#4142,#4143);
#3601=AXIS2_PLACEMENT_3D('',#5385,#4144,#4145);
#3602=AXIS2_PLACEMENT_3D('',#5386,#4146,#4147);
#3603=AXIS2_PLACEMENT_3D('',#5388,#4148,#4149);
#3604=AXIS2_PLACEMENT_3D('',#5391,#4151,#4152);
#3605=AXIS2_PLACEMENT_3D('',#5392,#4153,#4154);
#3606=AXIS2_PLACEMENT_3D('',#5394,#4155,#4156);
#3607=AXIS2_PLACEMENT_3D('',#5397,#4158,#4159);
#3608=AXIS2_PLACEMENT_3D('',#5398,#4160,#4161);
#3609=AXIS2_PLACEMENT_3D('',#5400,#4162,#4163);
#3610=AXIS2_PLACEMENT_3D('',#5403,#4165,#4166);
#3611=AXIS2_PLACEMENT_3D('',#5404,#4167,#4168);
#3612=AXIS2_PLACEMENT_3D('',#5406,#4169,#4170);
#3613=AXIS2_PLACEMENT_3D('',#5409,#4172,#4173);
#3614=AXIS2_PLACEMENT_3D('',#5410,#4174,#4175);
#3615=AXIS2_PLACEMENT_3D('',#5412,#4176,#4177);
#3616=AXIS2_PLACEMENT_3D('',#5415,#4179,#4180);
#3617=AXIS2_PLACEMENT_3D('',#5416,#4181,#4182);
#3618=AXIS2_PLACEMENT_3D('',#5418,#4183,#4184);
#3619=AXIS2_PLACEMENT_3D('',#5421,#4186,#4187);
#3620=AXIS2_PLACEMENT_3D('',#5422,#4188,#4189);
#3621=AXIS2_PLACEMENT_3D('',#5424,#4190,#4191);
#3622=AXIS2_PLACEMENT_3D('',#5425,#4192,#4193);
#3623=AXIS2_PLACEMENT_3D('',#5427,#4194,#4195);
#3624=AXIS2_PLACEMENT_3D('',#5429,#4196,#4197);
#3625=AXIS2_PLACEMENT_3D('',#5430,#4198,#4199);
#3626=AXIS2_PLACEMENT_3D('',#5432,#4200,#4201);
#3627=AXIS2_PLACEMENT_3D('',#5434,#4203,#4204);
#3628=AXIS2_PLACEMENT_3D('',#5435,#4205,#4206);
#3629=AXIS2_PLACEMENT_3D('',#5438,#4208,#4209);
#3630=AXIS2_PLACEMENT_3D('',#5439,#4210,#4211);
#3631=AXIS2_PLACEMENT_3D('',#5442,#4213,#4214);
#3632=AXIS2_PLACEMENT_3D('',#5443,#4215,#4216);
#3633=AXIS2_PLACEMENT_3D('',#5445,#4217,#4218);
#3634=AXIS2_PLACEMENT_3D('',#5448,#4220,#4221);
#3635=AXIS2_PLACEMENT_3D('',#5449,#4222,#4223);
#3636=AXIS2_PLACEMENT_3D('',#5450,#4224,#4225);
#3637=AXIS2_PLACEMENT_3D('',#5451,#4226,#4227);
#3638=AXIS2_PLACEMENT_3D('',#5452,#4228,#4229);
#3639=AXIS2_PLACEMENT_3D('',#5454,#4230,#4231);
#3640=AXIS2_PLACEMENT_3D('',#5457,#4233,#4234);
#3641=AXIS2_PLACEMENT_3D('',#5458,#4235,#4236);
#3642=AXIS2_PLACEMENT_3D('',#5460,#4237,#4238);
#3643=AXIS2_PLACEMENT_3D('',#5463,#4240,#4241);
#3644=AXIS2_PLACEMENT_3D('',#5464,#4242,#4243);
#3645=AXIS2_PLACEMENT_3D('',#5466,#4244,#4245);
#3646=AXIS2_PLACEMENT_3D('',#5469,#4247,#4248);
#3647=AXIS2_PLACEMENT_3D('',#5470,#4249,#4250);
#3648=AXIS2_PLACEMENT_3D('',#5472,#4251,#4252);
#3649=AXIS2_PLACEMENT_3D('',#5475,#4254,#4255);
#3650=AXIS2_PLACEMENT_3D('',#5476,#4256,#4257);
#3651=AXIS2_PLACEMENT_3D('',#5478,#4258,#4259);
#3652=AXIS2_PLACEMENT_3D('',#5481,#4261,#4262);
#3653=AXIS2_PLACEMENT_3D('',#5482,#4263,#4264);
#3654=AXIS2_PLACEMENT_3D('',#5484,#4265,#4266);
#3655=AXIS2_PLACEMENT_3D('',#5487,#4268,#4269);
#3656=AXIS2_PLACEMENT_3D('',#5488,#4270,#4271);
#3657=AXIS2_PLACEMENT_3D('',#5490,#4272,#4273);
#3658=AXIS2_PLACEMENT_3D('',#5491,#4274,#4275);
#3659=AXIS2_PLACEMENT_3D('',#5493,#4276,#4277);
#3660=AXIS2_PLACEMENT_3D('',#5495,#4278,#4279);
#3661=AXIS2_PLACEMENT_3D('',#5496,#4280,#4281);
#3662=AXIS2_PLACEMENT_3D('',#5498,#4282,#4283);
#3663=AXIS2_PLACEMENT_3D('',#5500,#4285,#4286);
#3664=AXIS2_PLACEMENT_3D('',#5501,#4287,#4288);
#3665=AXIS2_PLACEMENT_3D('',#5504,#4290,#4291);
#3666=AXIS2_PLACEMENT_3D('',#5505,#4292,#4293);
#3667=AXIS2_PLACEMENT_3D('',#5508,#4295,#4296);
#3668=AXIS2_PLACEMENT_3D('',#5509,#4297,#4298);
#3669=AXIS2_PLACEMENT_3D('',#5511,#4299,#4300);
#3670=AXIS2_PLACEMENT_3D('',#5514,#4302,#4303);
#3671=AXIS2_PLACEMENT_3D('',#5515,#4304,#4305);
#3672=AXIS2_PLACEMENT_3D('',#5516,#4306,#4307);
#3673=AXIS2_PLACEMENT_3D('',#5517,#4308,#4309);
#3674=AXIS2_PLACEMENT_3D('',#5518,#4310,#4311);
#3675=AXIS2_PLACEMENT_3D('',#5532,#4318,#4319);
#3676=AXIS2_PLACEMENT_3D('',#5533,#4320,#4321);
#3677=AXIS2_PLACEMENT_3D('',#5547,#4328,#4329);
#3678=AXIS2_PLACEMENT_3D('',#5548,#4330,#4331);
#3679=AXIS2_PLACEMENT_3D('',#5551,#4334,#4335);
#3680=AXIS2_PLACEMENT_3D('',#5553,#4337,#4338);
#3681=AXIS2_PLACEMENT_3D('',#5555,#4340,#4341);
#3682=AXIS2_PLACEMENT_3D('',#5557,#4343,#4344);
#3683=AXIS2_PLACEMENT_3D('',#5559,#4346,#4347);
#3684=AXIS2_PLACEMENT_3D('',#5560,#4348,#4349);
#3685=AXIS2_PLACEMENT_3D('',#5563,#4351,#4352);
#3686=AXIS2_PLACEMENT_3D('',#5564,#4353,#4354);
#3687=AXIS2_PLACEMENT_3D('',#5566,#4355,#4356);
#3688=AXIS2_PLACEMENT_3D('',#5568,#4357,#4358);
#3689=AXIS2_PLACEMENT_3D('',#5569,#4359,#4360);
#3690=AXIS2_PLACEMENT_3D('',#5571,#4362,#4363);
#3691=AXIS2_PLACEMENT_3D('',#5573,#4364,#4365);
#3692=AXIS2_PLACEMENT_3D('',#5575,#4367,#4368);
#3693=AXIS2_PLACEMENT_3D('',#5577,#4369,#4370);
#3694=AXIS2_PLACEMENT_3D('',#5579,#4372,#4373);
#3695=AXIS2_PLACEMENT_3D('',#5581,#4374,#4375);
#3696=AXIS2_PLACEMENT_3D('',#5582,#4376,#4377);
#3697=AXIS2_PLACEMENT_3D('',#5584,#4379,#4380);
#3698=AXIS2_PLACEMENT_3D('',#5585,#4381,#4382);
#3699=AXIS2_PLACEMENT_3D('',#5599,#4389,#4390);
#3700=AXIS2_PLACEMENT_3D('',#5600,#4391,#4392);
#3701=AXIS2_PLACEMENT_3D('',#5606,#4396,#4397);
#3702=AXIS2_PLACEMENT_3D('',#5610,#4400,#4401);
#3703=AXIS2_PLACEMENT_3D('',#5614,#4404,#4405);
#3704=AXIS2_PLACEMENT_3D('',#5618,#4408,#4409);
#3705=AXIS2_PLACEMENT_3D('',#5622,#4412,#4413);
#3706=AXIS2_PLACEMENT_3D('',#5624,#4415,#4416);
#3707=AXIS2_PLACEMENT_3D('',#5625,#4417,#4418);
#3708=AXIS2_PLACEMENT_3D('',#5628,#4420,#4421);
#3709=AXIS2_PLACEMENT_3D('',#5629,#4422,#4423);
#3710=AXIS2_PLACEMENT_3D('',#5630,#4424,#4425);
#3711=AXIS2_PLACEMENT_3D('',#5631,#4426,#4427);
#3712=AXIS2_PLACEMENT_3D('',#5640,#4432,#4433);
#3713=AXIS2_PLACEMENT_3D('',#5646,#4437,#4438);
#3714=AXIS2_PLACEMENT_3D('',#5652,#4442,#4443);
#3715=AXIS2_PLACEMENT_3D('',#5655,#4446,#4447);
#3716=AXIS2_PLACEMENT_3D('',#5656,#4448,#4449);
#3717=AXIS2_PLACEMENT_3D('',#5658,#4450,#4451);
#3718=AXIS2_PLACEMENT_3D('',#5659,#4452,#4453);
#3719=AXIS2_PLACEMENT_3D('',#5662,#4455,#4456);
#3720=AXIS2_PLACEMENT_3D('',#5663,#4457,#4458);
#3721=AXIS2_PLACEMENT_3D('',#5664,#4459,#4460);
#3722=AXIS2_PLACEMENT_3D('',#5665,#4461,#4462);
#3723=AXIS2_PLACEMENT_3D('',#5666,#4463,#4464);
#3724=AXIS2_PLACEMENT_3D('',#5668,#4465,#4466);
#3725=AXIS2_PLACEMENT_3D('',#5671,#4468,#4469);
#3726=AXIS2_PLACEMENT_3D('',#5672,#4470,#4471);
#3727=AXIS2_PLACEMENT_3D('',#5674,#4472,#4473);
#3728=AXIS2_PLACEMENT_3D('',#5675,#4474,#4475);
#3729=AXIS2_PLACEMENT_3D('',#5677,#4476,#4477);
#3730=AXIS2_PLACEMENT_3D('',#5680,#4479,#4480);
#3731=AXIS2_PLACEMENT_3D('',#5681,#4481,#4482);
#3732=AXIS2_PLACEMENT_3D('',#5683,#4483,#4484);
#3733=AXIS2_PLACEMENT_3D('',#5684,#4485,#4486);
#3734=AXIS2_PLACEMENT_3D('',#5686,#4487,#4488);
#3735=AXIS2_PLACEMENT_3D('',#5689,#4490,#4491);
#3736=AXIS2_PLACEMENT_3D('',#5690,#4492,#4493);
#3737=AXIS2_PLACEMENT_3D('',#5692,#4494,#4495);
#3738=AXIS2_PLACEMENT_3D('',#5693,#4496,#4497);
#3739=AXIS2_PLACEMENT_3D('',#5695,#4498,#4499);
#3740=AXIS2_PLACEMENT_3D('',#5698,#4501,#4502);
#3741=AXIS2_PLACEMENT_3D('',#5699,#4503,#4504);
#3742=AXIS2_PLACEMENT_3D('',#5701,#4505,#4506);
#3743=AXIS2_PLACEMENT_3D('',#5702,#4507,#4508);
#3744=AXIS2_PLACEMENT_3D('',#5704,#4509,#4510);
#3745=AXIS2_PLACEMENT_3D('',#5706,#4512,#4513);
#3746=AXIS2_PLACEMENT_3D('',#5708,#4514,#4515);
#3747=AXIS2_PLACEMENT_3D('',#5710,#4517,#4518);
#3748=AXIS2_PLACEMENT_3D('',#5712,#4519,#4520);
#3749=AXIS2_PLACEMENT_3D('',#5714,#4522,#4523);
#3750=AXIS2_PLACEMENT_3D('',#5716,#4524,#4525);
#3751=AXIS2_PLACEMENT_3D('',#5718,#4527,#4528);
#3752=AXIS2_PLACEMENT_3D('',#5720,#4529,#4530);
#3753=AXIS2_PLACEMENT_3D('',#5723,#4532,#4533);
#3754=AXIS2_PLACEMENT_3D('',#5724,#4534,#4535);
#3755=AXIS2_PLACEMENT_3D('',#5726,#4536,#4537);
#3756=AXIS2_PLACEMENT_3D('',#5727,#4538,#4539);
#3757=AXIS2_PLACEMENT_3D('',#5729,#4540,#4541);
#3758=AXIS2_PLACEMENT_3D('',#5732,#4543,#4544);
#3759=AXIS2_PLACEMENT_3D('',#5733,#4545,#4546);
#3760=AXIS2_PLACEMENT_3D('',#5735,#4547,#4548);
#3761=AXIS2_PLACEMENT_3D('',#5737,#4550,#4551);
#3762=AXIS2_PLACEMENT_3D('',#5739,#4552,#4553);
#3763=AXIS2_PLACEMENT_3D('',#5742,#4555,#4556);
#3764=AXIS2_PLACEMENT_3D('',#5743,#4557,#4558);
#3765=AXIS2_PLACEMENT_3D('',#5752,#4563,#4564);
#3766=AXIS2_PLACEMENT_3D('',#5758,#4568,#4569);
#3767=AXIS2_PLACEMENT_3D('',#5764,#4573,#4574);
#3768=AXIS2_PLACEMENT_3D('',#5767,#4577,#4578);
#3769=AXIS2_PLACEMENT_3D('',#5768,#4579,#4580);
#3770=AXIS2_PLACEMENT_3D('',#5769,#4581,#4582);
#3771=AXIS2_PLACEMENT_3D('',#5770,#4583,#4584);
#3772=AXIS2_PLACEMENT_3D('',#5772,#4585,#4586);
#3773=AXIS2_PLACEMENT_3D('',#5775,#4588,#4589);
#3774=AXIS2_PLACEMENT_3D('',#5776,#4590,#4591);
#3775=AXIS2_PLACEMENT_3D('',#5778,#4592,#4593);
#3776=AXIS2_PLACEMENT_3D('',#5781,#4595,#4596);
#3777=AXIS2_PLACEMENT_3D('',#5782,#4597,#4598);
#3778=AXIS2_PLACEMENT_3D('',#5784,#4599,#4600);
#3779=AXIS2_PLACEMENT_3D('',#5787,#4602,#4603);
#3780=AXIS2_PLACEMENT_3D('',#5788,#4604,#4605);
#3781=AXIS2_PLACEMENT_3D('',#5790,#4606,#4607);
#3782=AXIS2_PLACEMENT_3D('',#5793,#4609,#4610);
#3783=AXIS2_PLACEMENT_3D('',#5794,#4611,#4612);
#3784=AXIS2_PLACEMENT_3D('',#5796,#4613,#4614);
#3785=AXIS2_PLACEMENT_3D('',#5799,#4616,#4617);
#3786=AXIS2_PLACEMENT_3D('',#5800,#4618,#4619);
#3787=AXIS2_PLACEMENT_3D('',#5802,#4620,#4621);
#3788=AXIS2_PLACEMENT_3D('',#5805,#4623,#4624);
#3789=AXIS2_PLACEMENT_3D('',#5806,#4625,#4626);
#3790=AXIS2_PLACEMENT_3D('',#5808,#4627,#4628);
#3791=AXIS2_PLACEMENT_3D('',#5811,#4630,#4631);
#3792=AXIS2_PLACEMENT_3D('',#5812,#4632,#4633);
#3793=AXIS2_PLACEMENT_3D('',#5821,#4638,#4639);
#3794=AXIS2_PLACEMENT_3D('',#5827,#4643,#4644);
#3795=AXIS2_PLACEMENT_3D('',#5833,#4648,#4649);
#3796=AXIS2_PLACEMENT_3D('',#5836,#4652,#4653);
#3797=AXIS2_PLACEMENT_3D('',#5837,#4654,#4655);
#3798=AXIS2_PLACEMENT_3D('',#5838,#4656,#4657);
#3799=AXIS2_PLACEMENT_3D('',#5839,#4658,#4659);
#3800=AXIS2_PLACEMENT_3D('',#5841,#4660,#4661);
#3801=AXIS2_PLACEMENT_3D('',#5844,#4663,#4664);
#3802=AXIS2_PLACEMENT_3D('',#5845,#4665,#4666);
#3803=AXIS2_PLACEMENT_3D('',#5847,#4667,#4668);
#3804=AXIS2_PLACEMENT_3D('',#5848,#4669,#4670);
#3805=AXIS2_PLACEMENT_3D('',#5862,#4677,#4678);
#3806=AXIS2_PLACEMENT_3D('',#5863,#4679,#4680);
#3807=AXIS2_PLACEMENT_3D('',#5869,#4684,#4685);
#3808=AXIS2_PLACEMENT_3D('',#5873,#4688,#4689);
#3809=AXIS2_PLACEMENT_3D('',#5877,#4692,#4693);
#3810=AXIS2_PLACEMENT_3D('',#5881,#4696,#4697);
#3811=AXIS2_PLACEMENT_3D('',#5885,#4700,#4701);
#3812=AXIS2_PLACEMENT_3D('',#5887,#4703,#4704);
#3813=AXIS2_PLACEMENT_3D('',#5888,#4705,#4706);
#3814=AXIS2_PLACEMENT_3D('',#5891,#4708,#4709);
#3815=AXIS2_PLACEMENT_3D('',#5892,#4710,#4711);
#3816=AXIS2_PLACEMENT_3D('',#5895,#4713,#4714);
#3817=AXIS2_PLACEMENT_3D('',#5896,#4715,#4716);
#3818=AXIS2_PLACEMENT_3D('',#5897,#4717,#4718);
#3819=AXIS2_PLACEMENT_3D('',#5898,#4719,#4720);
#3820=AXIS2_PLACEMENT_3D('',#5899,#4721,#4722);
#3821=AXIS2_PLACEMENT_3D('',#5901,#4723,#4724);
#3822=AXIS2_PLACEMENT_3D('',#5904,#4726,#4727);
#3823=AXIS2_PLACEMENT_3D('',#5905,#4728,#4729);
#3824=AXIS2_PLACEMENT_3D('',#5907,#4730,#4731);
#3825=AXIS2_PLACEMENT_3D('',#5908,#4732,#4733);
#3826=AXIS2_PLACEMENT_3D('',#5922,#4740,#4741);
#3827=AXIS2_PLACEMENT_3D('',#5923,#4742,#4743);
#3828=AXIS2_PLACEMENT_3D('',#5937,#4750,#4751);
#3829=AXIS2_PLACEMENT_3D('',#5938,#4752,#4753);
#3830=AXIS2_PLACEMENT_3D('',#5941,#4756,#4757);
#3831=AXIS2_PLACEMENT_3D('',#5943,#4759,#4760);
#3832=AXIS2_PLACEMENT_3D('',#5945,#4762,#4763);
#3833=AXIS2_PLACEMENT_3D('',#5947,#4765,#4766);
#3834=AXIS2_PLACEMENT_3D('',#5949,#4768,#4769);
#3835=AXIS2_PLACEMENT_3D('',#5950,#4770,#4771);
#3836=AXIS2_PLACEMENT_3D('',#5952,#4772,#4773);
#3837=AXIS2_PLACEMENT_3D('',#5953,#4774,#4775);
#3838=AXIS2_PLACEMENT_3D('',#5956,#4777,#4778);
#3839=AXIS2_PLACEMENT_3D('',#5957,#4779,#4780);
#3840=AXIS2_PLACEMENT_3D('',#5959,#4781,#4782);
#3841=AXIS2_PLACEMENT_3D('',#5960,#4783,#4784);
#3842=AXIS2_PLACEMENT_3D('',#5962,#4786,#4787);
#3843=AXIS2_PLACEMENT_3D('',#5964,#4788,#4789);
#3844=AXIS2_PLACEMENT_3D('',#5966,#4791,#4792);
#3845=AXIS2_PLACEMENT_3D('',#5968,#4793,#4794);
#3846=AXIS2_PLACEMENT_3D('',#5969,#4795,#4796);
#3847=AXIS2_PLACEMENT_3D('',#5971,#4798,#4799);
#3848=AXIS2_PLACEMENT_3D('',#5972,#4800,#4801);
#3849=AXIS2_PLACEMENT_3D('',#5974,#4802,#4803);
#3850=AXIS2_PLACEMENT_3D('',#5976,#4804,#4805);
#3851=AXIS2_PLACEMENT_3D('',#5977,#4806,#4807);
#3852=AXIS2_PLACEMENT_3D('',#5979,#4808,#4809);
#3853=AXIS2_PLACEMENT_3D('',#5981,#4811,#4812);
#3854=AXIS2_PLACEMENT_3D('',#5983,#4813,#4814);
#3855=AXIS2_PLACEMENT_3D('',#5984,#4815,#4816);
#3856=AXIS2_PLACEMENT_3D('',#5986,#4817,#4818);
#3857=AXIS2_PLACEMENT_3D('',#5988,#4820,#4821);
#3858=AXIS2_PLACEMENT_3D('',#5990,#4822,#4823);
#3859=AXIS2_PLACEMENT_3D('',#5991,#4824,#4825);
#3860=AXIS2_PLACEMENT_3D('',#5993,#4827,#4828);
#3861=AXIS2_PLACEMENT_3D('',#5994,#4829,#4830);
#3862=AXIS2_PLACEMENT_3D('',#5995,#4831,#4832);
#3863=AXIS2_PLACEMENT_3D('',#5996,#4833,#4834);
#3864=AXIS2_PLACEMENT_3D('',#5998,#4835,#4836);
#3865=AXIS2_PLACEMENT_3D('',#5999,#4837,#4838);
#3866=AXIS2_PLACEMENT_3D('',#6001,#4839,#4840);
#3867=AXIS2_PLACEMENT_3D('',#6003,#4842,#4843);
#3868=AXIS2_PLACEMENT_3D('',#6005,#4844,#4845);
#3869=AXIS2_PLACEMENT_3D('',#6007,#4847,#4848);
#3870=AXIS2_PLACEMENT_3D('',#6009,#4849,#4850);
#3871=AXIS2_PLACEMENT_3D('',#6011,#4852,#4853);
#3872=AXIS2_PLACEMENT_3D('',#6013,#4854,#4855);
#3873=AXIS2_PLACEMENT_3D('',#6014,#4856,#4857);
#3874=AXIS2_PLACEMENT_3D('',#6016,#4858,#4859);
#3875=AXIS2_PLACEMENT_3D('',#6018,#4861,#4862);
#3876=AXIS2_PLACEMENT_3D('',#6020,#4863,#4864);
#3877=AXIS2_PLACEMENT_3D('',#6022,#4866,#4867);
#3878=AXIS2_PLACEMENT_3D('',#6024,#4868,#4869);
#3879=AXIS2_PLACEMENT_3D('',#6026,#4871,#4872);
#3880=AXIS2_PLACEMENT_3D('',#6027,#4873,#4874);
#3881=AXIS2_PLACEMENT_3D('',#6036,#4879,#4880);
#3882=AXIS2_PLACEMENT_3D('',#6042,#4884,#4885);
#3883=AXIS2_PLACEMENT_3D('',#6048,#4889,#4890);
#3884=AXIS2_PLACEMENT_3D('',#6054,#4894,#4895);
#3885=AXIS2_PLACEMENT_3D('',#6060,#4899,#4900);
#3886=AXIS2_PLACEMENT_3D('',#6063,#4903,#4904);
#3887=AXIS2_PLACEMENT_3D('',#6064,#4905,#4906);
#3888=AXIS2_PLACEMENT_3D('',#6065,#4907,#4908);
#3889=AXIS2_PLACEMENT_3D('',#6066,#4909,#4910);
#3890=AXIS2_PLACEMENT_3D('',#6067,#4911,#4912);
#3891=AXIS2_PLACEMENT_3D('',#6068,#4913,#4914);
#3892=AXIS2_PLACEMENT_3D('',#6069,#4915,#4916);
#3893=AXIS2_PLACEMENT_3D('',#6070,#4917,#4918);
#3894=AXIS2_PLACEMENT_3D('',#6071,#4919,#4920);
#3895=AXIS2_PLACEMENT_3D('',#6072,#4921,#4922);
#3896=AXIS2_PLACEMENT_3D('',#6073,#4923,#4924);
#3897=AXIS2_PLACEMENT_3D('',#6074,#4925,#4926);
#3898=AXIS2_PLACEMENT_3D('',#6075,#4927,#4928);
#3899=AXIS2_PLACEMENT_3D('',#6076,#4929,#4930);
#3900=AXIS2_PLACEMENT_3D('',#6077,#4931,#4932);
#3901=AXIS2_PLACEMENT_3D('',#6078,#4933,#4934);
#3902=AXIS2_PLACEMENT_3D('',#6079,#4935,#4936);
#3903=AXIS2_PLACEMENT_3D('',#6080,#4937,#4938);
#3904=AXIS2_PLACEMENT_3D('',#6081,#4939,#4940);
#3905=DIRECTION('axis',(0.,0.,1.));
#3906=DIRECTION('refdir',(1.,0.,0.));
#3907=DIRECTION('axis',(0.,0.,1.));
#3908=DIRECTION('refdir',(1.,0.,0.));
#3909=DIRECTION('center_axis',(0.,0.,1.));
#3910=DIRECTION('ref_axis',(1.,0.,0.));
#3911=DIRECTION('center_axis',(0.,0.,1.));
#3912=DIRECTION('ref_axis',(1.,0.,0.));
#3913=DIRECTION('',(0.,0.,1.));
#3914=DIRECTION('center_axis',(0.,0.,-1.));
#3915=DIRECTION('ref_axis',(1.,0.,0.));
#3916=DIRECTION('center_axis',(0.,0.,1.));
#3917=DIRECTION('ref_axis',(1.,0.,0.));
#3918=DIRECTION('center_axis',(0.,0.,1.));
#3919=DIRECTION('ref_axis',(1.,0.,0.));
#3920=DIRECTION('center_axis',(0.,0.,1.));
#3921=DIRECTION('ref_axis',(1.,0.,0.));
#3922=DIRECTION('',(0.,0.,1.));
#3923=DIRECTION('center_axis',(0.,0.,-1.));
#3924=DIRECTION('ref_axis',(1.,0.,0.));
#3925=DIRECTION('center_axis',(0.,0.,1.));
#3926=DIRECTION('ref_axis',(1.,0.,0.));
#3927=DIRECTION('center_axis',(0.,0.,1.));
#3928=DIRECTION('ref_axis',(1.,0.,0.));
#3929=DIRECTION('center_axis',(0.,0.,1.));
#3930=DIRECTION('ref_axis',(1.,0.,0.));
#3931=DIRECTION('',(0.,0.,1.));
#3932=DIRECTION('center_axis',(0.,0.,-1.));
#3933=DIRECTION('ref_axis',(1.,0.,0.));
#3934=DIRECTION('center_axis',(0.,0.,1.));
#3935=DIRECTION('ref_axis',(1.,0.,0.));
#3936=DIRECTION('center_axis',(0.,0.,1.));
#3937=DIRECTION('ref_axis',(1.,0.,0.));
#3938=DIRECTION('center_axis',(0.,0.,1.));
#3939=DIRECTION('ref_axis',(1.,0.,0.));
#3940=DIRECTION('',(0.,0.,1.));
#3941=DIRECTION('center_axis',(0.,0.,-1.));
#3942=DIRECTION('ref_axis',(1.,0.,0.));
#3943=DIRECTION('center_axis',(0.,0.,1.));
#3944=DIRECTION('ref_axis',(1.,0.,0.));
#3945=DIRECTION('center_axis',(0.,0.,1.));
#3946=DIRECTION('ref_axis',(1.,0.,0.));
#3947=DIRECTION('',(0.,0.,1.));
#3948=DIRECTION('center_axis',(0.,0.,-1.));
#3949=DIRECTION('ref_axis',(1.,0.,0.));
#3950=DIRECTION('center_axis',(0.,0.,1.));
#3951=DIRECTION('ref_axis',(1.,0.,0.));
#3952=DIRECTION('',(0.,0.,1.));
#3953=DIRECTION('center_axis',(0.,0.,-1.));
#3954=DIRECTION('ref_axis',(1.,0.,0.));
#3955=DIRECTION('center_axis',(0.,0.,1.));
#3956=DIRECTION('ref_axis',(1.,0.,0.));
#3957=DIRECTION('',(0.,0.,1.));
#3958=DIRECTION('center_axis',(0.,0.,-1.));
#3959=DIRECTION('ref_axis',(1.,0.,0.));
#3960=DIRECTION('center_axis',(0.,0.,1.));
#3961=DIRECTION('ref_axis',(1.,0.,0.));
#3962=DIRECTION('center_axis',(0.,0.,1.));
#3963=DIRECTION('ref_axis',(1.,0.,0.));
#3964=DIRECTION('',(0.,0.,1.));
#3965=DIRECTION('center_axis',(0.,0.,-1.));
#3966=DIRECTION('ref_axis',(1.,0.,0.));
#3967=DIRECTION('center_axis',(0.,0.,1.));
#3968=DIRECTION('ref_axis',(1.,0.,0.));
#3969=DIRECTION('center_axis',(0.,0.,1.));
#3970=DIRECTION('ref_axis',(1.,0.,0.));
#3971=DIRECTION('center_axis',(0.,0.,1.));
#3972=DIRECTION('ref_axis',(1.,0.,0.));
#3973=DIRECTION('',(0.,0.,1.));
#3974=DIRECTION('center_axis',(0.,0.,-1.));
#3975=DIRECTION('ref_axis',(1.,0.,0.));
#3976=DIRECTION('center_axis',(0.,0.,1.));
#3977=DIRECTION('ref_axis',(1.,0.,0.));
#3978=DIRECTION('center_axis',(0.,0.,1.));
#3979=DIRECTION('ref_axis',(1.,0.,0.));
#3980=DIRECTION('center_axis',(0.,0.,1.));
#3981=DIRECTION('ref_axis',(1.,0.,0.));
#3982=DIRECTION('',(0.,0.,1.));
#3983=DIRECTION('center_axis',(0.,0.,-1.));
#3984=DIRECTION('ref_axis',(1.,0.,0.));
#3985=DIRECTION('center_axis',(0.,0.,1.));
#3986=DIRECTION('ref_axis',(1.,0.,0.));
#3987=DIRECTION('center_axis',(0.,0.,1.));
#3988=DIRECTION('ref_axis',(1.,0.,0.));
#3989=DIRECTION('center_axis',(0.,0.,1.));
#3990=DIRECTION('ref_axis',(1.,0.,0.));
#3991=DIRECTION('',(0.,0.,1.));
#3992=DIRECTION('center_axis',(0.,0.,-1.));
#3993=DIRECTION('ref_axis',(1.,0.,0.));
#3994=DIRECTION('center_axis',(0.,0.,1.));
#3995=DIRECTION('ref_axis',(1.,0.,0.));
#3996=DIRECTION('center_axis',(0.,0.,1.));
#3997=DIRECTION('ref_axis',(1.,0.,0.));
#3998=DIRECTION('',(0.,0.,1.));
#3999=DIRECTION('center_axis',(0.,0.,-1.));
#4000=DIRECTION('ref_axis',(1.,0.,0.));
#4001=DIRECTION('center_axis',(0.,0.,1.));
#4002=DIRECTION('ref_axis',(1.,0.,0.));
#4003=DIRECTION('',(0.,0.,1.));
#4004=DIRECTION('center_axis',(0.,0.,-1.));
#4005=DIRECTION('ref_axis',(1.,0.,0.));
#4006=DIRECTION('center_axis',(0.,0.,1.));
#4007=DIRECTION('ref_axis',(1.,0.,0.));
#4008=DIRECTION('',(0.,0.,1.));
#4009=DIRECTION('center_axis',(0.,0.,-1.));
#4010=DIRECTION('ref_axis',(1.,0.,0.));
#4011=DIRECTION('center_axis',(0.,0.,1.));
#4012=DIRECTION('ref_axis',(1.,0.,0.));
#4013=DIRECTION('center_axis',(0.,0.,1.));
#4014=DIRECTION('ref_axis',(1.,0.,0.));
#4015=DIRECTION('',(0.,0.,1.));
#4016=DIRECTION('center_axis',(0.,0.,-1.));
#4017=DIRECTION('ref_axis',(1.,0.,0.));
#4018=DIRECTION('center_axis',(0.,0.,1.));
#4019=DIRECTION('ref_axis',(1.,0.,0.));
#4020=DIRECTION('center_axis',(0.,0.,1.));
#4021=DIRECTION('ref_axis',(1.,0.,0.));
#4022=DIRECTION('',(0.,0.,1.));
#4023=DIRECTION('center_axis',(0.,0.,-1.));
#4024=DIRECTION('ref_axis',(1.,0.,0.));
#4025=DIRECTION('center_axis',(0.,0.,1.));
#4026=DIRECTION('ref_axis',(1.,0.,0.));
#4027=DIRECTION('center_axis',(0.,0.,1.));
#4028=DIRECTION('ref_axis',(1.,0.,0.));
#4029=DIRECTION('',(0.,0.,1.));
#4030=DIRECTION('center_axis',(0.,0.,-1.));
#4031=DIRECTION('ref_axis',(1.,0.,0.));
#4032=DIRECTION('center_axis',(0.,0.,1.));
#4033=DIRECTION('ref_axis',(1.,0.,0.));
#4034=DIRECTION('center_axis',(0.,0.,1.));
#4035=DIRECTION('ref_axis',(1.,0.,0.));
#4036=DIRECTION('',(0.,0.,1.));
#4037=DIRECTION('center_axis',(0.,0.,-1.));
#4038=DIRECTION('ref_axis',(1.,0.,0.));
#4039=DIRECTION('center_axis',(1.,0.,0.));
#4040=DIRECTION('ref_axis',(0.,0.,-1.));
#4041=DIRECTION('center_axis',(1.,0.,0.));
#4042=DIRECTION('ref_axis',(0.,0.,-1.));
#4043=DIRECTION('',(1.,0.,0.));
#4044=DIRECTION('center_axis',(-1.,0.,0.));
#4045=DIRECTION('ref_axis',(0.,0.,-1.));
#4046=DIRECTION('center_axis',(1.,0.,0.));
#4047=DIRECTION('ref_axis',(0.,0.,-1.));
#4048=DIRECTION('center_axis',(1.,0.,0.));
#4049=DIRECTION('ref_axis',(0.,0.,-1.));
#4050=DIRECTION('center_axis',(1.,0.,0.));
#4051=DIRECTION('ref_axis',(0.,0.,-1.));
#4052=DIRECTION('center_axis',(1.,0.,0.));
#4053=DIRECTION('ref_axis',(0.,0.,-1.));
#4054=DIRECTION('',(1.,0.,0.));
#4055=DIRECTION('center_axis',(-1.,0.,0.));
#4056=DIRECTION('ref_axis',(0.,0.,-1.));
#4057=DIRECTION('center_axis',(1.,0.,0.));
#4058=DIRECTION('ref_axis',(0.,0.,-1.));
#4059=DIRECTION('center_axis',(1.,0.,0.));
#4060=DIRECTION('ref_axis',(0.,0.,-1.));
#4061=DIRECTION('center_axis',(1.,0.,0.));
#4062=DIRECTION('ref_axis',(0.,0.,-1.));
#4063=DIRECTION('center_axis',(1.,0.,0.));
#4064=DIRECTION('ref_axis',(0.,0.,-1.));
#4065=DIRECTION('',(1.,0.,0.));
#4066=DIRECTION('center_axis',(-1.,0.,0.));
#4067=DIRECTION('ref_axis',(0.,0.,-1.));
#4068=DIRECTION('center_axis',(1.,0.,0.));
#4069=DIRECTION('ref_axis',(0.,0.,-1.));
#4070=DIRECTION('center_axis',(1.,0.,0.));
#4071=DIRECTION('ref_axis',(0.,0.,-1.));
#4072=DIRECTION('center_axis',(1.,0.,0.));
#4073=DIRECTION('ref_axis',(0.,0.,-1.));
#4074=DIRECTION('center_axis',(1.,0.,0.));
#4075=DIRECTION('ref_axis',(0.,0.,-1.));
#4076=DIRECTION('',(1.,0.,0.));
#4077=DIRECTION('center_axis',(1.,0.,0.));
#4078=DIRECTION('ref_axis',(0.,0.,-1.));
#4079=DIRECTION('center_axis',(1.,0.,0.));
#4080=DIRECTION('ref_axis',(0.,0.,-1.));
#4081=DIRECTION('center_axis',(-1.,0.,0.));
#4082=DIRECTION('ref_axis',(0.,0.,-1.));
#4083=DIRECTION('center_axis',(1.,0.,0.));
#4084=DIRECTION('ref_axis',(0.,0.,-1.));
#4085=DIRECTION('center_axis',(1.,0.,0.));
#4086=DIRECTION('ref_axis',(0.,0.,-1.));
#4087=DIRECTION('',(1.,0.,0.));
#4088=DIRECTION('center_axis',(1.,0.,0.));
#4089=DIRECTION('ref_axis',(0.,0.,-1.));
#4090=DIRECTION('center_axis',(1.,0.,0.));
#4091=DIRECTION('ref_axis',(0.,0.,-1.));
#4092=DIRECTION('center_axis',(-1.,0.,0.));
#4093=DIRECTION('ref_axis',(0.,0.,-1.));
#4094=DIRECTION('center_axis',(1.,0.,0.));
#4095=DIRECTION('ref_axis',(0.,0.,-1.));
#4096=DIRECTION('center_axis',(1.,0.,0.));
#4097=DIRECTION('ref_axis',(0.,0.,-1.));
#4098=DIRECTION('',(1.,0.,0.));
#4099=DIRECTION('center_axis',(1.,0.,0.));
#4100=DIRECTION('ref_axis',(0.,0.,-1.));
#4101=DIRECTION('center_axis',(1.,0.,0.));
#4102=DIRECTION('ref_axis',(0.,0.,-1.));
#4103=DIRECTION('center_axis',(-1.,0.,0.));
#4104=DIRECTION('ref_axis',(0.,0.,-1.));
#4105=DIRECTION('center_axis',(1.,0.,0.));
#4106=DIRECTION('ref_axis',(0.,0.,-1.));
#4107=DIRECTION('',(1.,0.,0.));
#4108=DIRECTION('',(1.,0.,0.));
#4109=DIRECTION('',(1.,0.,0.));
#4110=DIRECTION('center_axis',(1.,0.,0.));
#4111=DIRECTION('ref_axis',(0.,0.,-1.));
#4112=DIRECTION('',(1.,0.,0.));
#4113=DIRECTION('',(1.,0.,0.));
#4114=DIRECTION('',(1.,0.,0.));
#4115=DIRECTION('center_axis',(1.,0.,0.));
#4116=DIRECTION('ref_axis',(0.,0.,-1.));
#4117=DIRECTION('',(1.,0.,0.));
#4118=DIRECTION('',(1.,0.,0.));
#4119=DIRECTION('',(1.,0.,0.));
#4120=DIRECTION('center_axis',(0.,1.,0.));
#4121=DIRECTION('ref_axis',(-1.,0.,0.));
#4122=DIRECTION('',(-1.,0.,0.));
#4123=DIRECTION('',(0.,0.,1.));
#4124=DIRECTION('',(-1.,0.,0.));
#4125=DIRECTION('',(0.,0.,1.));
#4126=DIRECTION('center_axis',(1.,0.,0.));
#4127=DIRECTION('ref_axis',(0.,1.,0.));
#4128=DIRECTION('',(0.,1.,0.));
#4129=DIRECTION('',(0.,1.,0.));
#4130=DIRECTION('',(0.,0.,1.));
#4131=DIRECTION('center_axis',(0.,-1.,0.));
#4132=DIRECTION('ref_axis',(1.,0.,0.));
#4133=DIRECTION('',(1.,0.,0.));
#4134=DIRECTION('',(1.,0.,0.));
#4135=DIRECTION('',(0.,0.,1.));
#4136=DIRECTION('center_axis',(-1.,0.,0.));
#4137=DIRECTION('ref_axis',(0.,-1.,0.));
#4138=DIRECTION('',(0.,-1.,0.));
#4139=DIRECTION('',(0.,-1.,0.));
#4140=DIRECTION('center_axis',(0.,0.,1.));
#4141=DIRECTION('ref_axis',(1.,0.,0.));
#4142=DIRECTION('center_axis',(0.,0.,1.));
#4143=DIRECTION('ref_axis',(1.,0.,0.));
#4144=DIRECTION('axis',(0.,0.,1.));
#4145=DIRECTION('refdir',(1.,0.,0.));
#4146=DIRECTION('center_axis',(1.,0.,0.));
#4147=DIRECTION('ref_axis',(0.,0.,-1.));
#4148=DIRECTION('center_axis',(1.,0.,0.));
#4149=DIRECTION('ref_axis',(0.,0.,-1.));
#4150=DIRECTION('',(1.,0.,0.));
#4151=DIRECTION('center_axis',(-1.,0.,0.));
#4152=DIRECTION('ref_axis',(0.,0.,-1.));
#4153=DIRECTION('center_axis',(1.,0.,0.));
#4154=DIRECTION('ref_axis',(0.,0.,-1.));
#4155=DIRECTION('center_axis',(1.,0.,0.));
#4156=DIRECTION('ref_axis',(0.,0.,-1.));
#4157=DIRECTION('',(1.,0.,0.));
#4158=DIRECTION('center_axis',(-1.,0.,0.));
#4159=DIRECTION('ref_axis',(0.,0.,-1.));
#4160=DIRECTION('center_axis',(1.,0.,0.));
#4161=DIRECTION('ref_axis',(0.,0.,-1.));
#4162=DIRECTION('center_axis',(1.,0.,0.));
#4163=DIRECTION('ref_axis',(0.,0.,-1.));
#4164=DIRECTION('',(1.,0.,0.));
#4165=DIRECTION('center_axis',(-1.,0.,0.));
#4166=DIRECTION('ref_axis',(0.,0.,-1.));
#4167=DIRECTION('center_axis',(1.,0.,0.));
#4168=DIRECTION('ref_axis',(0.,0.,-1.));
#4169=DIRECTION('center_axis',(1.,0.,0.));
#4170=DIRECTION('ref_axis',(0.,0.,-1.));
#4171=DIRECTION('',(1.,0.,0.));
#4172=DIRECTION('center_axis',(-1.,0.,0.));
#4173=DIRECTION('ref_axis',(0.,0.,-1.));
#4174=DIRECTION('center_axis',(1.,0.,0.));
#4175=DIRECTION('ref_axis',(0.,0.,-1.));
#4176=DIRECTION('center_axis',(1.,0.,0.));
#4177=DIRECTION('ref_axis',(0.,0.,-1.));
#4178=DIRECTION('',(1.,0.,0.));
#4179=DIRECTION('center_axis',(-1.,0.,0.));
#4180=DIRECTION('ref_axis',(0.,0.,-1.));
#4181=DIRECTION('center_axis',(1.,0.,0.));
#4182=DIRECTION('ref_axis',(0.,0.,-1.));
#4183=DIRECTION('center_axis',(1.,0.,0.));
#4184=DIRECTION('ref_axis',(0.,0.,-1.));
#4185=DIRECTION('',(1.,0.,0.));
#4186=DIRECTION('center_axis',(-1.,0.,0.));
#4187=DIRECTION('ref_axis',(0.,0.,-1.));
#4188=DIRECTION('center_axis',(1.,0.,0.));
#4189=DIRECTION('ref_axis',(0.,0.,-1.));
#4190=DIRECTION('center_axis',(1.,0.,0.));
#4191=DIRECTION('ref_axis',(0.,0.,-1.));
#4192=DIRECTION('center_axis',(1.,0.,0.));
#4193=DIRECTION('ref_axis',(0.,0.,-1.));
#4194=DIRECTION('center_axis',(1.,0.,0.));
#4195=DIRECTION('ref_axis',(0.,0.,-1.));
#4196=DIRECTION('center_axis',(-1.,0.,0.));
#4197=DIRECTION('ref_axis',(0.,0.,-1.));
#4198=DIRECTION('center_axis',(1.,0.,0.));
#4199=DIRECTION('ref_axis',(0.,0.,-1.));
#4200=DIRECTION('center_axis',(1.,0.,0.));
#4201=DIRECTION('ref_axis',(0.,0.,-1.));
#4202=DIRECTION('',(-1.,0.,0.));
#4203=DIRECTION('center_axis',(1.,0.,0.));
#4204=DIRECTION('ref_axis',(0.,0.,-1.));
#4205=DIRECTION('center_axis',(1.,0.,0.));
#4206=DIRECTION('ref_axis',(0.,0.,-1.));
#4207=DIRECTION('',(-1.,0.,0.));
#4208=DIRECTION('center_axis',(-1.,0.,0.));
#4209=DIRECTION('ref_axis',(0.,0.,-1.));
#4210=DIRECTION('center_axis',(1.,0.,0.));
#4211=DIRECTION('ref_axis',(0.,0.,-1.));
#4212=DIRECTION('',(-1.,0.,0.));
#4213=DIRECTION('center_axis',(-1.,0.,0.));
#4214=DIRECTION('ref_axis',(0.,0.,-1.));
#4215=DIRECTION('center_axis',(1.,0.,0.));
#4216=DIRECTION('ref_axis',(0.,0.,-1.));
#4217=DIRECTION('center_axis',(1.,0.,0.));
#4218=DIRECTION('ref_axis',(0.,0.,-1.));
#4219=DIRECTION('',(-1.,0.,0.));
#4220=DIRECTION('center_axis',(1.,0.,0.));
#4221=DIRECTION('ref_axis',(0.,0.,-1.));
#4222=DIRECTION('center_axis',(1.,0.,0.));
#4223=DIRECTION('ref_axis',(0.,0.,-1.));
#4224=DIRECTION('center_axis',(1.,0.,0.));
#4225=DIRECTION('ref_axis',(0.,0.,-1.));
#4226=DIRECTION('axis',(0.,0.,1.));
#4227=DIRECTION('refdir',(1.,0.,0.));
#4228=DIRECTION('center_axis',(1.,0.,0.));
#4229=DIRECTION('ref_axis',(0.,0.,-1.));
#4230=DIRECTION('center_axis',(1.,0.,0.));
#4231=DIRECTION('ref_axis',(0.,0.,-1.));
#4232=DIRECTION('',(1.,0.,0.));
#4233=DIRECTION('center_axis',(-1.,0.,0.));
#4234=DIRECTION('ref_axis',(0.,0.,-1.));
#4235=DIRECTION('center_axis',(1.,0.,0.));
#4236=DIRECTION('ref_axis',(0.,0.,-1.));
#4237=DIRECTION('center_axis',(1.,0.,0.));
#4238=DIRECTION('ref_axis',(0.,0.,-1.));
#4239=DIRECTION('',(1.,0.,0.));
#4240=DIRECTION('center_axis',(-1.,0.,0.));
#4241=DIRECTION('ref_axis',(0.,0.,-1.));
#4242=DIRECTION('center_axis',(1.,0.,0.));
#4243=DIRECTION('ref_axis',(0.,0.,-1.));
#4244=DIRECTION('center_axis',(1.,0.,0.));
#4245=DIRECTION('ref_axis',(0.,0.,-1.));
#4246=DIRECTION('',(1.,0.,0.));
#4247=DIRECTION('center_axis',(-1.,0.,0.));
#4248=DIRECTION('ref_axis',(0.,0.,-1.));
#4249=DIRECTION('center_axis',(1.,0.,0.));
#4250=DIRECTION('ref_axis',(0.,0.,-1.));
#4251=DIRECTION('center_axis',(1.,0.,0.));
#4252=DIRECTION('ref_axis',(0.,0.,-1.));
#4253=DIRECTION('',(1.,0.,0.));
#4254=DIRECTION('center_axis',(-1.,0.,0.));
#4255=DIRECTION('ref_axis',(0.,0.,-1.));
#4256=DIRECTION('center_axis',(1.,0.,0.));
#4257=DIRECTION('ref_axis',(0.,0.,-1.));
#4258=DIRECTION('center_axis',(1.,0.,0.));
#4259=DIRECTION('ref_axis',(0.,0.,-1.));
#4260=DIRECTION('',(1.,0.,0.));
#4261=DIRECTION('center_axis',(-1.,0.,0.));
#4262=DIRECTION('ref_axis',(0.,0.,-1.));
#4263=DIRECTION('center_axis',(1.,0.,0.));
#4264=DIRECTION('ref_axis',(0.,0.,-1.));
#4265=DIRECTION('center_axis',(1.,0.,0.));
#4266=DIRECTION('ref_axis',(0.,0.,-1.));
#4267=DIRECTION('',(1.,0.,0.));
#4268=DIRECTION('center_axis',(-1.,0.,0.));
#4269=DIRECTION('ref_axis',(0.,0.,-1.));
#4270=DIRECTION('center_axis',(1.,0.,0.));
#4271=DIRECTION('ref_axis',(0.,0.,-1.));
#4272=DIRECTION('center_axis',(1.,0.,0.));
#4273=DIRECTION('ref_axis',(0.,0.,-1.));
#4274=DIRECTION('center_axis',(1.,0.,0.));
#4275=DIRECTION('ref_axis',(0.,0.,-1.));
#4276=DIRECTION('center_axis',(1.,0.,0.));
#4277=DIRECTION('ref_axis',(0.,0.,-1.));
#4278=DIRECTION('center_axis',(-1.,0.,0.));
#4279=DIRECTION('ref_axis',(0.,0.,-1.));
#4280=DIRECTION('center_axis',(1.,0.,0.));
#4281=DIRECTION('ref_axis',(0.,0.,-1.));
#4282=DIRECTION('center_axis',(1.,0.,0.));
#4283=DIRECTION('ref_axis',(0.,0.,-1.));
#4284=DIRECTION('',(-1.,0.,0.));
#4285=DIRECTION('center_axis',(1.,0.,0.));
#4286=DIRECTION('ref_axis',(0.,0.,-1.));
#4287=DIRECTION('center_axis',(1.,0.,0.));
#4288=DIRECTION('ref_axis',(0.,0.,-1.));
#4289=DIRECTION('',(-1.,0.,0.));
#4290=DIRECTION('center_axis',(-1.,0.,0.));
#4291=DIRECTION('ref_axis',(0.,0.,-1.));
#4292=DIRECTION('center_axis',(1.,0.,0.));
#4293=DIRECTION('ref_axis',(0.,0.,-1.));
#4294=DIRECTION('',(-1.,0.,0.));
#4295=DIRECTION('center_axis',(-1.,0.,0.));
#4296=DIRECTION('ref_axis',(0.,0.,-1.));
#4297=DIRECTION('center_axis',(1.,0.,0.));
#4298=DIRECTION('ref_axis',(0.,0.,-1.));
#4299=DIRECTION('center_axis',(1.,0.,0.));
#4300=DIRECTION('ref_axis',(0.,0.,-1.));
#4301=DIRECTION('',(-1.,0.,0.));
#4302=DIRECTION('center_axis',(1.,0.,0.));
#4303=DIRECTION('ref_axis',(0.,0.,-1.));
#4304=DIRECTION('center_axis',(1.,0.,0.));
#4305=DIRECTION('ref_axis',(0.,0.,-1.));
#4306=DIRECTION('center_axis',(1.,0.,0.));
#4307=DIRECTION('ref_axis',(0.,0.,-1.));
#4308=DIRECTION('axis',(0.,0.,1.));
#4309=DIRECTION('refdir',(1.,0.,0.));
#4310=DIRECTION('center_axis',(0.,1.,0.));
#4311=DIRECTION('ref_axis',(1.,0.,0.));
#4312=DIRECTION('',(-0.5,0.,0.866025403784439));
#4313=DIRECTION('',(-1.,0.,-3.29650746237182E-16));
#4314=DIRECTION('',(-0.5,0.,-0.866025403784439));
#4315=DIRECTION('',(0.5,0.,-0.866025403784438));
#4316=DIRECTION('',(1.,0.,0.));
#4317=DIRECTION('',(0.5,0.,0.866025403784439));
#4318=DIRECTION('center_axis',(0.,-1.,0.));
#4319=DIRECTION('ref_axis',(1.,0.,0.));
#4320=DIRECTION('center_axis',(0.,1.,0.));
#4321=DIRECTION('ref_axis',(1.,0.,0.));
#4322=DIRECTION('',(0.5,0.,-0.866025403784439));
#4323=DIRECTION('',(-0.5,0.,-0.866025403784439));
#4324=DIRECTION('',(-1.,0.,0.));
#4325=DIRECTION('',(-0.5,0.,0.866025403784438));
#4326=DIRECTION('',(0.5,0.,0.866025403784439));
#4327=DIRECTION('',(1.,0.,3.29650746237182E-16));
#4328=DIRECTION('center_axis',(0.,1.,0.));
#4329=DIRECTION('ref_axis',(1.,0.,0.));
#4330=DIRECTION('center_axis',(-3.29650746237182E-16,0.,1.));
#4331=DIRECTION('ref_axis',(1.,0.,3.29650746237182E-16));
#4332=DIRECTION('',(0.,-1.,0.));
#4333=DIRECTION('',(0.,1.,0.));
#4334=DIRECTION('center_axis',(-0.866025403784439,0.,0.5));
#4335=DIRECTION('ref_axis',(0.5,0.,0.866025403784439));
#4336=DIRECTION('',(0.,1.,0.));
#4337=DIRECTION('center_axis',(-0.866025403784439,0.,-0.5));
#4338=DIRECTION('ref_axis',(-0.5,0.,0.866025403784439));
#4339=DIRECTION('',(0.,1.,0.));
#4340=DIRECTION('center_axis',(0.,0.,-1.));
#4341=DIRECTION('ref_axis',(-1.,0.,0.));
#4342=DIRECTION('',(0.,1.,0.));
#4343=DIRECTION('center_axis',(0.866025403784439,0.,-0.5));
#4344=DIRECTION('ref_axis',(-0.5,0.,-0.866025403784439));
#4345=DIRECTION('',(0.,1.,0.));
#4346=DIRECTION('center_axis',(0.866025403784439,0.,0.5));
#4347=DIRECTION('ref_axis',(0.5,0.,-0.866025403784439));
#4348=DIRECTION('center_axis',(0.,-1.,0.));
#4349=DIRECTION('ref_axis',(1.,0.,0.));
#4350=DIRECTION('',(0.,1.,0.));
#4351=DIRECTION('center_axis',(0.,-1.,0.));
#4352=DIRECTION('ref_axis',(1.,0.,0.));
#4353=DIRECTION('center_axis',(0.,1.,0.));
#4354=DIRECTION('ref_axis',(0.,0.,1.));
#4355=DIRECTION('center_axis',(0.,-1.,0.));
#4356=DIRECTION('ref_axis',(1.,0.,0.));
#4357=DIRECTION('center_axis',(0.,-1.,0.));
#4358=DIRECTION('ref_axis',(1.,0.,0.));
#4359=DIRECTION('center_axis',(0.,-1.,0.));
#4360=DIRECTION('ref_axis',(1.,0.,0.));
#4361=DIRECTION('',(0.707106781186547,0.707106781186548,8.65956056235493E-17));
#4362=DIRECTION('center_axis',(0.,-1.,0.));
#4363=DIRECTION('ref_axis',(1.,0.,0.));
#4364=DIRECTION('center_axis',(0.,-1.,0.));
#4365=DIRECTION('ref_axis',(1.,0.,0.));
#4366=DIRECTION('',(0.,1.,0.));
#4367=DIRECTION('center_axis',(0.,1.,0.));
#4368=DIRECTION('ref_axis',(1.,0.,0.));
#4369=DIRECTION('center_axis',(0.,-1.,0.));
#4370=DIRECTION('ref_axis',(1.,0.,0.));
#4371=DIRECTION('',(-0.707106781186547,0.707106781186548,-8.65956056235493E-17));
#4372=DIRECTION('center_axis',(0.,-1.,0.));
#4373=DIRECTION('ref_axis',(0.,0.,-1.));
#4374=DIRECTION('center_axis',(0.,-1.,0.));
#4375=DIRECTION('ref_axis',(1.,0.,0.));
#4376=DIRECTION('center_axis',(0.,-1.,0.));
#4377=DIRECTION('ref_axis',(1.,0.,0.));
#4378=DIRECTION('',(0.,1.,0.));
#4379=DIRECTION('axis',(0.,0.,1.));
#4380=DIRECTION('refdir',(1.,0.,0.));
#4381=DIRECTION('center_axis',(1.,0.,0.));
#4382=DIRECTION('ref_axis',(0.,0.,-1.));
#4383=DIRECTION('',(0.,0.5,0.866025403784439));
#4384=DIRECTION('',(0.,1.,-4.39534328316243E-16));
#4385=DIRECTION('',(0.,0.5,-0.866025403784439));
#4386=DIRECTION('',(0.,-0.5,-0.866025403784439));
#4387=DIRECTION('',(0.,-1.,0.));
#4388=DIRECTION('',(0.,-0.5,0.866025403784439));
#4389=DIRECTION('center_axis',(1.,0.,0.));
#4390=DIRECTION('ref_axis',(0.,0.,-1.));
#4391=DIRECTION('center_axis',(0.,-4.39534328316243E-16,-1.));
#4392=DIRECTION('ref_axis',(0.,1.,-4.39534328316243E-16));
#4393=DIRECTION('',(1.,0.,0.));
#4394=DIRECTION('',(0.,1.,-4.39534328316243E-16));
#4395=DIRECTION('',(1.,0.,0.));
#4396=DIRECTION('center_axis',(0.,-0.866025403784439,-0.5));
#4397=DIRECTION('ref_axis',(0.,0.5,-0.866025403784439));
#4398=DIRECTION('',(0.,0.5,-0.866025403784439));
#4399=DIRECTION('',(1.,0.,0.));
#4400=DIRECTION('center_axis',(0.,-0.866025403784439,0.5));
#4401=DIRECTION('ref_axis',(0.,-0.5,-0.866025403784439));
#4402=DIRECTION('',(0.,-0.5,-0.866025403784439));
#4403=DIRECTION('',(1.,0.,0.));
#4404=DIRECTION('center_axis',(0.,0.,1.));
#4405=DIRECTION('ref_axis',(0.,-1.,0.));
#4406=DIRECTION('',(0.,-1.,0.));
#4407=DIRECTION('',(1.,0.,0.));
#4408=DIRECTION('center_axis',(0.,0.866025403784439,0.5));
#4409=DIRECTION('ref_axis',(0.,-0.5,0.866025403784439));
#4410=DIRECTION('',(0.,-0.5,0.866025403784439));
#4411=DIRECTION('',(1.,0.,0.));
#4412=DIRECTION('center_axis',(0.,0.866025403784439,-0.5));
#4413=DIRECTION('ref_axis',(0.,0.5,0.866025403784439));
#4414=DIRECTION('',(0.,0.5,0.866025403784439));
#4415=DIRECTION('center_axis',(1.,0.,0.));
#4416=DIRECTION('ref_axis',(0.,0.,-1.));
#4417=DIRECTION('center_axis',(1.,0.,0.));
#4418=DIRECTION('ref_axis',(0.,0.,-1.));
#4419=DIRECTION('',(-1.,0.,0.));
#4420=DIRECTION('center_axis',(1.,0.,0.));
#4421=DIRECTION('ref_axis',(0.,0.,-1.));
#4422=DIRECTION('center_axis',(1.,0.,0.));
#4423=DIRECTION('ref_axis',(0.,0.,-1.));
#4424=DIRECTION('axis',(0.,0.,1.));
#4425=DIRECTION('refdir',(1.,0.,0.));
#4426=DIRECTION('center_axis',(0.,0.,-1.));
#4427=DIRECTION('ref_axis',(0.,1.,0.));
#4428=DIRECTION('',(0.,-1.,0.));
#4429=DIRECTION('',(1.,0.,0.));
#4430=DIRECTION('',(0.,1.,0.));
#4431=DIRECTION('',(1.,0.,0.));
#4432=DIRECTION('center_axis',(0.,-1.,0.));
#4433=DIRECTION('ref_axis',(0.,0.,-1.));
#4434=DIRECTION('',(0.,0.,1.));
#4435=DIRECTION('',(0.,0.,-1.));
#4436=DIRECTION('',(1.,0.,0.));
#4437=DIRECTION('center_axis',(0.,0.,1.));
#4438=DIRECTION('ref_axis',(0.,-1.,0.));
#4439=DIRECTION('',(0.,1.,0.));
#4440=DIRECTION('',(0.,-1.,0.));
#4441=DIRECTION('',(1.,0.,0.));
#4442=DIRECTION('center_axis',(0.,1.,0.));
#4443=DIRECTION('ref_axis',(0.,0.,1.));
#4444=DIRECTION('',(0.,0.,-1.));
#4445=DIRECTION('',(0.,0.,1.));
#4446=DIRECTION('center_axis',(1.,0.,0.));
#4447=DIRECTION('ref_axis',(0.,0.,-1.));
#4448=DIRECTION('center_axis',(1.,0.,0.));
#4449=DIRECTION('ref_axis',(0.,0.,-1.));
#4450=DIRECTION('center_axis',(1.,0.,0.));
#4451=DIRECTION('ref_axis',(0.,0.,-1.));
#4452=DIRECTION('center_axis',(1.,0.,0.));
#4453=DIRECTION('ref_axis',(0.,0.,-1.));
#4454=DIRECTION('',(-1.,0.,0.));
#4455=DIRECTION('center_axis',(1.,0.,0.));
#4456=DIRECTION('ref_axis',(0.,0.,-1.));
#4457=DIRECTION('center_axis',(1.,0.,0.));
#4458=DIRECTION('ref_axis',(0.,0.,-1.));
#4459=DIRECTION('axis',(0.,0.,1.));
#4460=DIRECTION('refdir',(1.,0.,0.));
#4461=DIRECTION('axis',(0.,0.,1.));
#4462=DIRECTION('refdir',(1.,0.,0.));
#4463=DIRECTION('center_axis',(0.,0.,1.));
#4464=DIRECTION('ref_axis',(1.,0.,0.));
#4465=DIRECTION('center_axis',(0.,0.,1.));
#4466=DIRECTION('ref_axis',(1.,0.,0.));
#4467=DIRECTION('',(0.,0.,1.));
#4468=DIRECTION('center_axis',(0.,0.,-1.));
#4469=DIRECTION('ref_axis',(1.,0.,0.));
#4470=DIRECTION('center_axis',(0.,0.,1.));
#4471=DIRECTION('ref_axis',(1.,0.,0.));
#4472=DIRECTION('center_axis',(0.,0.,1.));
#4473=DIRECTION('ref_axis',(1.,0.,0.));
#4474=DIRECTION('center_axis',(0.,0.,1.));
#4475=DIRECTION('ref_axis',(1.,0.,0.));
#4476=DIRECTION('center_axis',(0.,0.,1.));
#4477=DIRECTION('ref_axis',(1.,0.,0.));
#4478=DIRECTION('',(0.,0.,1.));
#4479=DIRECTION('center_axis',(0.,0.,-1.));
#4480=DIRECTION('ref_axis',(1.,0.,0.));
#4481=DIRECTION('center_axis',(0.,0.,1.));
#4482=DIRECTION('ref_axis',(1.,0.,0.));
#4483=DIRECTION('center_axis',(0.,0.,1.));
#4484=DIRECTION('ref_axis',(1.,0.,0.));
#4485=DIRECTION('center_axis',(0.,0.,1.));
#4486=DIRECTION('ref_axis',(1.,0.,0.));
#4487=DIRECTION('center_axis',(0.,0.,1.));
#4488=DIRECTION('ref_axis',(1.,0.,0.));
#4489=DIRECTION('',(0.,0.,1.));
#4490=DIRECTION('center_axis',(0.,0.,-1.));
#4491=DIRECTION('ref_axis',(1.,0.,0.));
#4492=DIRECTION('center_axis',(0.,0.,1.));
#4493=DIRECTION('ref_axis',(1.,0.,0.));
#4494=DIRECTION('center_axis',(0.,0.,1.));
#4495=DIRECTION('ref_axis',(1.,0.,0.));
#4496=DIRECTION('center_axis',(0.,0.,1.));
#4497=DIRECTION('ref_axis',(1.,0.,0.));
#4498=DIRECTION('center_axis',(0.,0.,1.));
#4499=DIRECTION('ref_axis',(1.,0.,0.));
#4500=DIRECTION('',(0.,0.,1.));
#4501=DIRECTION('center_axis',(0.,0.,-1.));
#4502=DIRECTION('ref_axis',(1.,0.,0.));
#4503=DIRECTION('center_axis',(0.,0.,1.));
#4504=DIRECTION('ref_axis',(1.,0.,0.));
#4505=DIRECTION('center_axis',(0.,0.,1.));
#4506=DIRECTION('ref_axis',(1.,0.,0.));
#4507=DIRECTION('center_axis',(0.,0.,1.));
#4508=DIRECTION('ref_axis',(1.,0.,0.));
#4509=DIRECTION('center_axis',(0.,0.,1.));
#4510=DIRECTION('ref_axis',(1.,0.,0.));
#4511=DIRECTION('',(0.,0.,1.));
#4512=DIRECTION('center_axis',(0.,0.,1.));
#4513=DIRECTION('ref_axis',(1.,0.,0.));
#4514=DIRECTION('center_axis',(0.,0.,1.));
#4515=DIRECTION('ref_axis',(1.,0.,0.));
#4516=DIRECTION('',(0.,0.,1.));
#4517=DIRECTION('center_axis',(0.,0.,1.));
#4518=DIRECTION('ref_axis',(1.,0.,0.));
#4519=DIRECTION('center_axis',(0.,0.,1.));
#4520=DIRECTION('ref_axis',(1.,0.,0.));
#4521=DIRECTION('',(0.,0.,1.));
#4522=DIRECTION('center_axis',(0.,0.,1.));
#4523=DIRECTION('ref_axis',(1.,0.,0.));
#4524=DIRECTION('center_axis',(0.,0.,1.));
#4525=DIRECTION('ref_axis',(1.,0.,0.));
#4526=DIRECTION('',(0.,0.,1.));
#4527=DIRECTION('center_axis',(0.,0.,1.));
#4528=DIRECTION('ref_axis',(1.,0.,0.));
#4529=DIRECTION('center_axis',(0.,0.,1.));
#4530=DIRECTION('ref_axis',(1.,0.,0.));
#4531=DIRECTION('',(0.,0.,1.));
#4532=DIRECTION('center_axis',(0.,0.,-1.));
#4533=DIRECTION('ref_axis',(1.,0.,0.));
#4534=DIRECTION('center_axis',(0.,0.,1.));
#4535=DIRECTION('ref_axis',(1.,0.,0.));
#4536=DIRECTION('center_axis',(0.,0.,1.));
#4537=DIRECTION('ref_axis',(1.,0.,0.));
#4538=DIRECTION('center_axis',(0.,0.,1.));
#4539=DIRECTION('ref_axis',(1.,0.,0.));
#4540=DIRECTION('center_axis',(0.,0.,1.));
#4541=DIRECTION('ref_axis',(1.,0.,0.));
#4542=DIRECTION('',(0.,0.,1.));
#4543=DIRECTION('center_axis',(0.,0.,-1.));
#4544=DIRECTION('ref_axis',(1.,0.,0.));
#4545=DIRECTION('center_axis',(0.,0.,1.));
#4546=DIRECTION('ref_axis',(1.,0.,0.));
#4547=DIRECTION('center_axis',(0.,0.,1.));
#4548=DIRECTION('ref_axis',(1.,0.,0.));
#4549=DIRECTION('',(0.,0.,1.));
#4550=DIRECTION('center_axis',(0.,0.,1.));
#4551=DIRECTION('ref_axis',(1.,0.,0.));
#4552=DIRECTION('center_axis',(0.,0.,1.));
#4553=DIRECTION('ref_axis',(1.,0.,0.));
#4554=DIRECTION('',(0.,0.,1.));
#4555=DIRECTION('center_axis',(0.,0.,-1.));
#4556=DIRECTION('ref_axis',(1.,0.,0.));
#4557=DIRECTION('center_axis',(0.,1.,0.));
#4558=DIRECTION('ref_axis',(-1.,0.,0.));
#4559=DIRECTION('',(-1.,0.,0.));
#4560=DIRECTION('',(0.,0.,1.));
#4561=DIRECTION('',(-1.,0.,0.));
#4562=DIRECTION('',(0.,0.,1.));
#4563=DIRECTION('center_axis',(1.,0.,0.));
#4564=DIRECTION('ref_axis',(0.,1.,0.));
#4565=DIRECTION('',(0.,1.,0.));
#4566=DIRECTION('',(0.,1.,0.));
#4567=DIRECTION('',(0.,0.,1.));
#4568=DIRECTION('center_axis',(0.,-1.,0.));
#4569=DIRECTION('ref_axis',(1.,0.,0.));
#4570=DIRECTION('',(1.,0.,0.));
#4571=DIRECTION('',(1.,0.,0.));
#4572=DIRECTION('',(0.,0.,1.));
#4573=DIRECTION('center_axis',(-1.,0.,0.));
#4574=DIRECTION('ref_axis',(0.,-1.,0.));
#4575=DIRECTION('',(0.,-1.,0.));
#4576=DIRECTION('',(0.,-1.,0.));
#4577=DIRECTION('center_axis',(0.,0.,1.));
#4578=DIRECTION('ref_axis',(1.,0.,0.));
#4579=DIRECTION('center_axis',(0.,0.,1.));
#4580=DIRECTION('ref_axis',(1.,0.,0.));
#4581=DIRECTION('axis',(0.,0.,1.));
#4582=DIRECTION('refdir',(1.,0.,0.));
#4583=DIRECTION('center_axis',(0.,0.,1.));
#4584=DIRECTION('ref_axis',(1.,0.,0.));
#4585=DIRECTION('center_axis',(0.,0.,1.));
#4586=DIRECTION('ref_axis',(1.,0.,0.));
#4587=DIRECTION('',(0.,0.,1.));
#4588=DIRECTION('center_axis',(0.,0.,-1.));
#4589=DIRECTION('ref_axis',(1.,0.,0.));
#4590=DIRECTION('center_axis',(0.,0.,1.));
#4591=DIRECTION('ref_axis',(1.,0.,0.));
#4592=DIRECTION('center_axis',(0.,0.,1.));
#4593=DIRECTION('ref_axis',(1.,0.,0.));
#4594=DIRECTION('',(0.,0.,1.));
#4595=DIRECTION('center_axis',(0.,0.,-1.));
#4596=DIRECTION('ref_axis',(1.,0.,0.));
#4597=DIRECTION('center_axis',(0.,0.,1.));
#4598=DIRECTION('ref_axis',(1.,0.,0.));
#4599=DIRECTION('center_axis',(0.,0.,1.));
#4600=DIRECTION('ref_axis',(1.,0.,0.));
#4601=DIRECTION('',(0.,0.,1.));
#4602=DIRECTION('center_axis',(0.,0.,-1.));
#4603=DIRECTION('ref_axis',(1.,0.,0.));
#4604=DIRECTION('center_axis',(0.,0.,1.));
#4605=DIRECTION('ref_axis',(1.,0.,0.));
#4606=DIRECTION('center_axis',(0.,0.,1.));
#4607=DIRECTION('ref_axis',(1.,0.,0.));
#4608=DIRECTION('',(0.,0.,1.));
#4609=DIRECTION('center_axis',(0.,0.,-1.));
#4610=DIRECTION('ref_axis',(1.,0.,0.));
#4611=DIRECTION('center_axis',(0.,0.,1.));
#4612=DIRECTION('ref_axis',(1.,0.,0.));
#4613=DIRECTION('center_axis',(0.,0.,1.));
#4614=DIRECTION('ref_axis',(1.,0.,0.));
#4615=DIRECTION('',(0.,0.,1.));
#4616=DIRECTION('center_axis',(0.,0.,-1.));
#4617=DIRECTION('ref_axis',(1.,0.,0.));
#4618=DIRECTION('center_axis',(0.,0.,1.));
#4619=DIRECTION('ref_axis',(1.,0.,0.));
#4620=DIRECTION('center_axis',(0.,0.,1.));
#4621=DIRECTION('ref_axis',(1.,0.,0.));
#4622=DIRECTION('',(0.,0.,1.));
#4623=DIRECTION('center_axis',(0.,0.,-1.));
#4624=DIRECTION('ref_axis',(1.,0.,0.));
#4625=DIRECTION('center_axis',(0.,0.,1.));
#4626=DIRECTION('ref_axis',(1.,0.,0.));
#4627=DIRECTION('center_axis',(0.,0.,1.));
#4628=DIRECTION('ref_axis',(1.,0.,0.));
#4629=DIRECTION('',(0.,0.,1.));
#4630=DIRECTION('center_axis',(0.,0.,-1.));
#4631=DIRECTION('ref_axis',(1.,0.,0.));
#4632=DIRECTION('center_axis',(0.,1.,0.));
#4633=DIRECTION('ref_axis',(-1.,0.,0.));
#4634=DIRECTION('',(-1.,0.,0.));
#4635=DIRECTION('',(0.,0.,1.));
#4636=DIRECTION('',(-1.,0.,0.));
#4637=DIRECTION('',(0.,0.,1.));
#4638=DIRECTION('center_axis',(1.,0.,0.));
#4639=DIRECTION('ref_axis',(0.,1.,0.));
#4640=DIRECTION('',(0.,1.,0.));
#4641=DIRECTION('',(0.,1.,0.));
#4642=DIRECTION('',(0.,0.,1.));
#4643=DIRECTION('center_axis',(0.,-1.,0.));
#4644=DIRECTION('ref_axis',(1.,0.,0.));
#4645=DIRECTION('',(1.,0.,0.));
#4646=DIRECTION('',(1.,0.,0.));
#4647=DIRECTION('',(0.,0.,1.));
#4648=DIRECTION('center_axis',(-1.,0.,0.));
#4649=DIRECTION('ref_axis',(0.,-1.,0.));
#4650=DIRECTION('',(0.,-1.,0.));
#4651=DIRECTION('',(0.,-1.,0.));
#4652=DIRECTION('center_axis',(0.,0.,1.));
#4653=DIRECTION('ref_axis',(1.,0.,0.));
#4654=DIRECTION('center_axis',(0.,0.,1.));
#4655=DIRECTION('ref_axis',(1.,0.,0.));
#4656=DIRECTION('axis',(0.,0.,1.));
#4657=DIRECTION('refdir',(1.,0.,0.));
#4658=DIRECTION('center_axis',(0.,0.,1.));
#4659=DIRECTION('ref_axis',(1.,0.,0.));
#4660=DIRECTION('center_axis',(0.,0.,1.));
#4661=DIRECTION('ref_axis',(1.,0.,0.));
#4662=DIRECTION('',(0.,0.,1.));
#4663=DIRECTION('center_axis',(0.,0.,-1.));
#4664=DIRECTION('ref_axis',(1.,0.,0.));
#4665=DIRECTION('center_axis',(0.,0.,1.));
#4666=DIRECTION('ref_axis',(1.,0.,0.));
#4667=DIRECTION('center_axis',(0.,0.,1.));
#4668=DIRECTION('ref_axis',(1.,0.,0.));
#4669=DIRECTION('center_axis',(0.,0.,1.));
#4670=DIRECTION('ref_axis',(1.,0.,0.));
#4671=DIRECTION('',(0.5,0.866025403784438,0.));
#4672=DIRECTION('',(1.,-3.29650746237182E-16,0.));
#4673=DIRECTION('',(0.499999999999999,-0.866025403784439,0.));
#4674=DIRECTION('',(-0.5,-0.866025403784439,0.));
#4675=DIRECTION('',(-1.,0.,0.));
#4676=DIRECTION('',(-0.5,0.866025403784438,0.));
#4677=DIRECTION('center_axis',(0.,0.,1.));
#4678=DIRECTION('ref_axis',(1.,0.,0.));
#4679=DIRECTION('center_axis',(-3.29650746237182E-16,-1.,0.));
#4680=DIRECTION('ref_axis',(1.,-3.29650746237182E-16,0.));
#4681=DIRECTION('',(0.,0.,1.));
#4682=DIRECTION('',(1.,-3.29650746237182E-16,0.));
#4683=DIRECTION('',(0.,0.,1.));
#4684=DIRECTION('center_axis',(-0.866025403784439,-0.499999999999999,0.));
#4685=DIRECTION('ref_axis',(0.499999999999999,-0.866025403784439,0.));
#4686=DIRECTION('',(0.499999999999999,-0.866025403784439,0.));
#4687=DIRECTION('',(0.,0.,1.));
#4688=DIRECTION('center_axis',(-0.866025403784439,0.5,0.));
#4689=DIRECTION('ref_axis',(-0.5,-0.866025403784439,0.));
#4690=DIRECTION('',(-0.5,-0.866025403784439,0.));
#4691=DIRECTION('',(0.,0.,1.));
#4692=DIRECTION('center_axis',(0.,1.,0.));
#4693=DIRECTION('ref_axis',(-1.,0.,0.));
#4694=DIRECTION('',(-1.,0.,0.));
#4695=DIRECTION('',(0.,0.,1.));
#4696=DIRECTION('center_axis',(0.866025403784438,0.5,0.));
#4697=DIRECTION('ref_axis',(-0.5,0.866025403784438,0.));
#4698=DIRECTION('',(-0.5,0.866025403784438,0.));
#4699=DIRECTION('',(0.,0.,1.));
#4700=DIRECTION('center_axis',(0.866025403784438,-0.5,0.));
#4701=DIRECTION('ref_axis',(0.5,0.866025403784438,0.));
#4702=DIRECTION('',(0.5,0.866025403784438,0.));
#4703=DIRECTION('center_axis',(0.,0.,1.));
#4704=DIRECTION('ref_axis',(1.,0.,0.));
#4705=DIRECTION('center_axis',(0.,0.,1.));
#4706=DIRECTION('ref_axis',(1.,0.,0.));
#4707=DIRECTION('',(0.,0.,-1.));
#4708=DIRECTION('center_axis',(0.,0.,-1.));
#4709=DIRECTION('ref_axis',(1.,0.,0.));
#4710=DIRECTION('center_axis',(0.,0.,1.));
#4711=DIRECTION('ref_axis',(1.,0.,0.));
#4712=DIRECTION('',(0.,0.,-1.));
#4713=DIRECTION('center_axis',(0.,0.,1.));
#4714=DIRECTION('ref_axis',(1.,0.,0.));
#4715=DIRECTION('center_axis',(0.,0.,1.));
#4716=DIRECTION('ref_axis',(1.,0.,0.));
#4717=DIRECTION('axis',(0.,0.,1.));
#4718=DIRECTION('refdir',(1.,0.,0.));
#4719=DIRECTION('axis',(0.,0.,1.));
#4720=DIRECTION('refdir',(1.,0.,0.));
#4721=DIRECTION('center_axis',(0.,1.,0.));
#4722=DIRECTION('ref_axis',(1.,0.,0.));
#4723=DIRECTION('center_axis',(0.,1.,0.));
#4724=DIRECTION('ref_axis',(1.,0.,0.));
#4725=DIRECTION('',(0.,1.,0.));
#4726=DIRECTION('center_axis',(0.,-1.,0.));
#4727=DIRECTION('ref_axis',(1.,0.,0.));
#4728=DIRECTION('center_axis',(0.,1.,0.));
#4729=DIRECTION('ref_axis',(1.,0.,0.));
#4730=DIRECTION('center_axis',(0.,1.,0.));
#4731=DIRECTION('ref_axis',(1.,0.,0.));
#4732=DIRECTION('center_axis',(0.,1.,0.));
#4733=DIRECTION('ref_axis',(1.,0.,0.));
#4734=DIRECTION('',(0.5,0.,-0.866025403784439));
#4735=DIRECTION('',(-0.5,0.,-0.866025403784439));
#4736=DIRECTION('',(-1.,0.,-1.60246890531964E-16));
#4737=DIRECTION('',(-0.5,0.,0.866025403784439));
#4738=DIRECTION('',(0.5,0.,0.866025403784439));
#4739=DIRECTION('',(1.,0.,1.60246890531964E-16));
#4740=DIRECTION('center_axis',(0.,-1.,0.));
#4741=DIRECTION('ref_axis',(1.,0.,0.));
#4742=DIRECTION('center_axis',(0.,1.,0.));
#4743=DIRECTION('ref_axis',(1.,0.,0.));
#4744=DIRECTION('',(0.5,0.,-0.866025403784439));
#4745=DIRECTION('',(1.,0.,1.60246890531964E-16));
#4746=DIRECTION('',(0.5,0.,0.866025403784439));
#4747=DIRECTION('',(-0.5,0.,0.866025403784439));
#4748=DIRECTION('',(-1.,0.,-1.60246890531964E-16));
#4749=DIRECTION('',(-0.5,0.,-0.866025403784439));
#4750=DIRECTION('center_axis',(0.,-1.,0.));
#4751=DIRECTION('ref_axis',(1.,0.,0.));
#4752=DIRECTION('center_axis',(-1.60246890531964E-16,0.,1.));
#4753=DIRECTION('ref_axis',(1.,0.,1.60246890531964E-16));
#4754=DIRECTION('',(0.,1.,0.));
#4755=DIRECTION('',(0.,1.,0.));
#4756=DIRECTION('center_axis',(-0.866025403784439,0.,0.5));
#4757=DIRECTION('ref_axis',(0.5,0.,0.866025403784439));
#4758=DIRECTION('',(0.,1.,0.));
#4759=DIRECTION('center_axis',(-0.866025403784439,0.,-0.5));
#4760=DIRECTION('ref_axis',(-0.5,0.,0.866025403784439));
#4761=DIRECTION('',(0.,1.,0.));
#4762=DIRECTION('center_axis',(1.60246890531964E-16,0.,-1.));
#4763=DIRECTION('ref_axis',(-1.,0.,-1.60246890531964E-16));
#4764=DIRECTION('',(0.,1.,0.));
#4765=DIRECTION('center_axis',(0.866025403784439,0.,-0.5));
#4766=DIRECTION('ref_axis',(-0.5,0.,-0.866025403784439));
#4767=DIRECTION('',(0.,1.,0.));
#4768=DIRECTION('center_axis',(0.866025403784439,0.,0.5));
#4769=DIRECTION('ref_axis',(0.5,0.,-0.866025403784439));
#4770=DIRECTION('center_axis',(0.,1.,0.));
#4771=DIRECTION('ref_axis',(0.,0.,1.));
#4772=DIRECTION('center_axis',(0.,-1.,0.));
#4773=DIRECTION('ref_axis',(1.,0.,0.));
#4774=DIRECTION('center_axis',(0.,-1.,0.));
#4775=DIRECTION('ref_axis',(1.,0.,0.));
#4776=DIRECTION('',(0.,1.,0.));
#4777=DIRECTION('center_axis',(0.,-1.,0.));
#4778=DIRECTION('ref_axis',(1.,0.,0.));
#4779=DIRECTION('center_axis',(0.,1.,0.));
#4780=DIRECTION('ref_axis',(0.,0.,1.));
#4781=DIRECTION('center_axis',(0.,-1.,0.));
#4782=DIRECTION('ref_axis',(1.,0.,0.));
#4783=DIRECTION('center_axis',(0.,-1.,0.));
#4784=DIRECTION('ref_axis',(1.,0.,0.));
#4785=DIRECTION('',(0.,1.,0.));
#4786=DIRECTION('center_axis',(0.,-1.,0.));
#4787=DIRECTION('ref_axis',(1.,0.,0.));
#4788=DIRECTION('center_axis',(0.,-1.,0.));
#4789=DIRECTION('ref_axis',(1.,0.,0.));
#4790=DIRECTION('',(0.,1.,0.));
#4791=DIRECTION('center_axis',(0.,-1.,0.));
#4792=DIRECTION('ref_axis',(0.,0.,-1.));
#4793=DIRECTION('center_axis',(0.,-1.,0.));
#4794=DIRECTION('ref_axis',(1.,0.,0.));
#4795=DIRECTION('center_axis',(0.,-1.,0.));
#4796=DIRECTION('ref_axis',(1.,0.,0.));
#4797=DIRECTION('',(0.,1.,0.));
#4798=DIRECTION('axis',(0.,0.,1.));
#4799=DIRECTION('refdir',(1.,0.,0.));
#4800=DIRECTION('center_axis',(0.,1.,0.));
#4801=DIRECTION('ref_axis',(0.,0.,1.));
#4802=DIRECTION('center_axis',(0.,-1.,0.));
#4803=DIRECTION('ref_axis',(1.,0.,0.));
#4804=DIRECTION('center_axis',(0.,-1.,0.));
#4805=DIRECTION('ref_axis',(1.,0.,0.));
#4806=DIRECTION('center_axis',(0.,-1.,0.));
#4807=DIRECTION('ref_axis',(1.,0.,0.));
#4808=DIRECTION('center_axis',(0.,-1.,0.));
#4809=DIRECTION('ref_axis',(1.,0.,0.));
#4810=DIRECTION('',(0.,1.,0.));
#4811=DIRECTION('center_axis',(0.,-1.,0.));
#4812=DIRECTION('ref_axis',(0.,0.,-1.));
#4813=DIRECTION('center_axis',(0.,-1.,0.));
#4814=DIRECTION('ref_axis',(1.,0.,0.));
#4815=DIRECTION('center_axis',(0.,-1.,0.));
#4816=DIRECTION('ref_axis',(1.,0.,0.));
#4817=DIRECTION('center_axis',(0.,-1.,0.));
#4818=DIRECTION('ref_axis',(1.,0.,0.));
#4819=DIRECTION('',(0.,1.,0.));
#4820=DIRECTION('center_axis',(0.,-1.,0.));
#4821=DIRECTION('ref_axis',(0.,0.,-1.));
#4822=DIRECTION('center_axis',(0.,-1.,0.));
#4823=DIRECTION('ref_axis',(1.,0.,0.));
#4824=DIRECTION('center_axis',(0.,-1.,0.));
#4825=DIRECTION('ref_axis',(1.,0.,0.));
#4826=DIRECTION('',(0.,1.,0.));
#4827=DIRECTION('',(0.,0.,1.));
#4828=DIRECTION('',(1.,0.,0.));
#4829=DIRECTION('',(0.,0.,1.));
#4830=DIRECTION('',(1.,0.,0.));
#4831=DIRECTION('axis',(0.,0.,1.));
#4832=DIRECTION('refdir',(1.,0.,0.));
#4833=DIRECTION('center_axis',(0.,1.,0.));
#4834=DIRECTION('ref_axis',(0.,0.,1.));
#4835=DIRECTION('center_axis',(0.,-1.,0.));
#4836=DIRECTION('ref_axis',(1.,0.,0.));
#4837=DIRECTION('center_axis',(0.,-1.,0.));
#4838=DIRECTION('ref_axis',(1.,0.,0.));
#4839=DIRECTION('center_axis',(0.,-1.,0.));
#4840=DIRECTION('ref_axis',(1.,0.,0.));
#4841=DIRECTION('',(0.707106781186547,0.707106781186548,8.65956056235493E-17));
#4842=DIRECTION('center_axis',(0.,-1.,0.));
#4843=DIRECTION('ref_axis',(1.,0.,0.));
#4844=DIRECTION('center_axis',(0.,-1.,0.));
#4845=DIRECTION('ref_axis',(1.,0.,0.));
#4846=DIRECTION('',(0.,1.,0.));
#4847=DIRECTION('center_axis',(0.,1.,0.));
#4848=DIRECTION('ref_axis',(1.,0.,0.));
#4849=DIRECTION('center_axis',(0.,-1.,0.));
#4850=DIRECTION('ref_axis',(1.,0.,0.));
#4851=DIRECTION('',(-0.707106781186547,0.707106781186548,-8.65956056235493E-17));
#4852=DIRECTION('center_axis',(0.,-1.,0.));
#4853=DIRECTION('ref_axis',(0.,0.,-1.));
#4854=DIRECTION('center_axis',(0.,-1.,0.));
#4855=DIRECTION('ref_axis',(1.,0.,0.));
#4856=DIRECTION('center_axis',(0.,1.,0.));
#4857=DIRECTION('ref_axis',(1.,0.,0.));
#4858=DIRECTION('center_axis',(0.,1.,0.));
#4859=DIRECTION('ref_axis',(1.,0.,0.));
#4860=DIRECTION('',(-0.447213595499958,0.894427190999916,-5.47678698264203E-17));
#4861=DIRECTION('center_axis',(0.,-1.,0.));
#4862=DIRECTION('ref_axis',(1.,0.,0.));
#4863=DIRECTION('center_axis',(0.,1.,0.));
#4864=DIRECTION('ref_axis',(1.,0.,0.));
#4865=DIRECTION('',(0.,1.,0.));
#4866=DIRECTION('center_axis',(0.,1.,0.));
#4867=DIRECTION('ref_axis',(1.,0.,0.));
#4868=DIRECTION('center_axis',(0.,-1.,0.));
#4869=DIRECTION('ref_axis',(1.,0.,0.));
#4870=DIRECTION('',(-0.707106781186547,0.707106781186548,-8.65956056235493E-17));
#4871=DIRECTION('center_axis',(0.,-1.,0.));
#4872=DIRECTION('ref_axis',(0.,0.,-1.));
#4873=DIRECTION('center_axis',(0.866025403784439,0.,-0.5));
#4874=DIRECTION('ref_axis',(0.5,0.,0.866025403784439));
#4875=DIRECTION('',(-0.5,0.,-0.866025403784439));
#4876=DIRECTION('',(0.,-1.,0.));
#4877=DIRECTION('',(0.5,0.,0.866025403784439));
#4878=DIRECTION('',(0.,-1.,0.));
#4879=DIRECTION('center_axis',(1.60246890531964E-16,0.,-1.));
#4880=DIRECTION('ref_axis',(1.,0.,1.60246890531964E-16));
#4881=DIRECTION('',(-1.,0.,-1.60246890531964E-16));
#4882=DIRECTION('',(0.,-1.,0.));
#4883=DIRECTION('',(1.,0.,1.60246890531964E-16));
#4884=DIRECTION('center_axis',(-0.866025403784439,0.,-0.5));
#4885=DIRECTION('ref_axis',(0.5,0.,-0.866025403784439));
#4886=DIRECTION('',(-0.5,0.,0.866025403784439));
#4887=DIRECTION('',(0.,-1.,0.));
#4888=DIRECTION('',(0.5,0.,-0.866025403784439));
#4889=DIRECTION('center_axis',(-0.866025403784439,0.,0.5));
#4890=DIRECTION('ref_axis',(-0.5,0.,-0.866025403784439));
#4891=DIRECTION('',(0.5,0.,0.866025403784439));
#4892=DIRECTION('',(0.,-1.,0.));
#4893=DIRECTION('',(-0.5,0.,-0.866025403784439));
#4894=DIRECTION('center_axis',(-1.60246890531964E-16,0.,1.));
#4895=DIRECTION('ref_axis',(-1.,0.,-1.60246890531964E-16));
#4896=DIRECTION('',(1.,0.,1.60246890531964E-16));
#4897=DIRECTION('',(0.,-1.,0.));
#4898=DIRECTION('',(-1.,0.,-1.60246890531964E-16));
#4899=DIRECTION('center_axis',(0.866025403784439,0.,0.5));
#4900=DIRECTION('ref_axis',(-0.5,0.,0.866025403784439));
#4901=DIRECTION('',(0.5,0.,-0.866025403784439));
#4902=DIRECTION('',(-0.5,0.,0.866025403784439));
#4903=DIRECTION('center_axis',(0.,1.,0.));
#4904=DIRECTION('ref_axis',(1.,0.,0.));
#4905=DIRECTION('center_axis',(0.,-1.,0.));
#4906=DIRECTION('ref_axis',(0.,0.,-1.));
#4907=DIRECTION('',(0.,0.,1.));
#4908=DIRECTION('',(1.,0.,0.));
#4909=DIRECTION('',(0.,0.,1.));
#4910=DIRECTION('',(1.,0.,0.));
#4911=DIRECTION('',(0.,0.,1.));
#4912=DIRECTION('',(1.,0.,0.));
#4913=DIRECTION('',(0.,-1.,2.22044604925031E-16));
#4914=DIRECTION('',(1.,0.,0.));
#4915=DIRECTION('',(0.,-1.,2.22044604925031E-16));
#4916=DIRECTION('',(1.,0.,0.));
#4917=DIRECTION('',(0.,-1.,2.22044604925031E-16));
#4918=DIRECTION('',(1.,0.,0.));
#4919=DIRECTION('',(0.,-1.,2.22044604925031E-16));
#4920=DIRECTION('',(1.,0.,0.));
#4921=DIRECTION('',(0.,-1.,2.22044604925031E-16));
#4922=DIRECTION('',(1.,0.,0.));
#4923=DIRECTION('',(0.,0.,1.));
#4924=DIRECTION('',(1.,0.,0.));
#4925=DIRECTION('',(0.,0.,1.));
#4926=DIRECTION('',(1.,0.,0.));
#4927=DIRECTION('',(0.,0.,1.));
#4928=DIRECTION('',(1.,0.,0.));
#4929=DIRECTION('',(0.,0.,1.));
#4930=DIRECTION('',(2.22044604925031E-16,-1.,0.));
#4931=DIRECTION('',(0.,0.,1.));
#4932=DIRECTION('',(1.,0.,0.));
#4933=DIRECTION('',(0.,0.,1.));
#4934=DIRECTION('',(-1.,1.22464679914735E-16,0.));
#4935=DIRECTION('',(0.,0.,1.));
#4936=DIRECTION('',(-1.,1.22464679914735E-16,0.));
#4937=DIRECTION('',(0.,0.,1.));
#4938=DIRECTION('',(1.,0.,0.));
#4939=DIRECTION('',(2.32753228758938E-16,-2.22044604925031E-16,0.999999999999998));
#4940=DIRECTION('',(1.,-9.03280718196864E-16,-3.38580766432819E-17));
#4941=CARTESIAN_POINT('',(0.,0.,0.));
#4942=CARTESIAN_POINT('',(0.,0.,0.));
#4943=CARTESIAN_POINT('Origin',(5.7,-2.4,0.8));
#4944=CARTESIAN_POINT('',(5.535,-2.4,0.8));
#4945=CARTESIAN_POINT('Origin',(5.7,-2.4,0.8));
#4946=CARTESIAN_POINT('',(5.535,-2.4,2.));
#4947=CARTESIAN_POINT('',(5.535,-2.4,0.8));
#4948=CARTESIAN_POINT('Origin',(5.7,-2.4,2.));
#4949=CARTESIAN_POINT('Origin',(5.7,-2.4,0.8));
#4950=CARTESIAN_POINT('Origin',(2.3,2.4,0.8));
#4951=CARTESIAN_POINT('',(2.135,2.4,0.8));
#4952=CARTESIAN_POINT('Origin',(2.3,2.4,0.8));
#4953=CARTESIAN_POINT('',(2.135,2.4,2.));
#4954=CARTESIAN_POINT('',(2.135,2.4,0.8));
#4955=CARTESIAN_POINT('Origin',(2.3,2.4,2.));
#4956=CARTESIAN_POINT('Origin',(2.3,2.4,0.8));
#4957=CARTESIAN_POINT('Origin',(2.3,-2.4,0.8));
#4958=CARTESIAN_POINT('',(2.135,-2.4,0.8));
#4959=CARTESIAN_POINT('Origin',(2.3,-2.4,0.8));
#4960=CARTESIAN_POINT('',(2.135,-2.4,2.));
#4961=CARTESIAN_POINT('',(2.135,-2.4,0.8));
#4962=CARTESIAN_POINT('Origin',(2.3,-2.4,2.));
#4963=CARTESIAN_POINT('Origin',(2.3,-2.4,0.8));
#4964=CARTESIAN_POINT('Origin',(5.7,2.4,0.8));
#4965=CARTESIAN_POINT('',(5.535,2.4,0.8));
#4966=CARTESIAN_POINT('Origin',(5.7,2.4,0.8));
#4967=CARTESIAN_POINT('',(5.535,2.4,2.));
#4968=CARTESIAN_POINT('',(5.535,2.4,0.8));
#4969=CARTESIAN_POINT('Origin',(5.7,2.4,2.));
#4970=CARTESIAN_POINT('Origin',(5.7,2.4,0.8));
#4971=CARTESIAN_POINT('Origin',(4.,-1.5,0.9));
#4972=CARTESIAN_POINT('',(4.,-1.7,1.22360679774998));
#4973=CARTESIAN_POINT('',(4.2,-1.5,1.3));
#4974=CARTESIAN_POINT('Ctrl Pts',(4.,-1.7,1.22360679774998));
#4975=CARTESIAN_POINT('Ctrl Pts',(4.02630182346442,-1.7,1.22360679774998));
#4976=CARTESIAN_POINT('Ctrl Pts',(4.05333179602069,-1.69456887761607,1.22872056892082));
#4977=CARTESIAN_POINT('Ctrl Pts',(4.10213335089966,-1.67398313783528,1.24474475389314));
#4978=CARTESIAN_POINT('Ctrl Pts',(4.12402433525871,-1.6588183772159,1.25527603224183));
#4979=CARTESIAN_POINT('Ctrl Pts',(4.15862698590242,-1.62421572657219,1.27377192701083));
#4980=CARTESIAN_POINT('Ctrl Pts',(4.17391823287771,-1.6022830144367,1.28316729552365));
#4981=CARTESIAN_POINT('Ctrl Pts',(4.19462445314031,-1.55320424736513,1.29633569102376));
#4982=CARTESIAN_POINT('Ctrl Pts',(4.2,-1.52601246699667,1.3));
#4983=CARTESIAN_POINT('Ctrl Pts',(4.2,-1.5,1.3));
#4984=CARTESIAN_POINT('',(3.8,-1.5,1.3));
#4985=CARTESIAN_POINT('Ctrl Pts',(3.8,-1.5,1.3));
#4986=CARTESIAN_POINT('Ctrl Pts',(3.8,-1.52601246699667,1.3));
#4987=CARTESIAN_POINT('Ctrl Pts',(3.80537554685969,-1.55320424736513,1.29633569102376));
#4988=CARTESIAN_POINT('Ctrl Pts',(3.82608176712229,-1.6022830144367,1.28316729552365));
#4989=CARTESIAN_POINT('Ctrl Pts',(3.84137301409757,-1.62421572657219,1.27377192701083));
#4990=CARTESIAN_POINT('Ctrl Pts',(3.87597566474129,-1.6588183772159,1.25527603224183));
#4991=CARTESIAN_POINT('Ctrl Pts',(3.89786664910035,-1.67398313783528,1.24474475389314));
#4992=CARTESIAN_POINT('Ctrl Pts',(3.94666820397931,-1.69456887761607,1.22872056892082));
#4993=CARTESIAN_POINT('Ctrl Pts',(3.97369817653558,-1.7,1.22360679774998));
#4994=CARTESIAN_POINT('Ctrl Pts',(4.,-1.7,1.22360679774998));
#4995=CARTESIAN_POINT('',(3.8,-1.5,2.));
#4996=CARTESIAN_POINT('',(3.8,-1.5,0.9));
#4997=CARTESIAN_POINT('Origin',(4.,-1.5,2.));
#4998=CARTESIAN_POINT('Ctrl Pts',(4.2,-1.5,1.3));
#4999=CARTESIAN_POINT('Ctrl Pts',(4.2,-1.47398753300333,1.3));
#5000=CARTESIAN_POINT('Ctrl Pts',(4.19462445314031,-1.44679575263487,1.29633569102376));
#5001=CARTESIAN_POINT('Ctrl Pts',(4.17391823287771,-1.3977169855633,1.28316729552365));
#5002=CARTESIAN_POINT('Ctrl Pts',(4.15862698590242,-1.37578427342781,1.27377192701083));
#5003=CARTESIAN_POINT('Ctrl Pts',(4.12402433525871,-1.3411816227841,1.25527603224183));
#5004=CARTESIAN_POINT('Ctrl Pts',(4.10213335089966,-1.32601686216472,1.24474475389314));
#5005=CARTESIAN_POINT('Ctrl Pts',(4.05333179602069,-1.30543112238393,1.22872056892082));
#5006=CARTESIAN_POINT('Ctrl Pts',(4.02630182346442,-1.3,1.22360679774998));
#5007=CARTESIAN_POINT('Ctrl Pts',(3.97369817653558,-1.3,1.22360679774998));
#5008=CARTESIAN_POINT('Ctrl Pts',(3.94666820397931,-1.30543112238393,1.22872056892082));
#5009=CARTESIAN_POINT('Ctrl Pts',(3.89786664910035,-1.32601686216472,1.24474475389314));
#5010=CARTESIAN_POINT('Ctrl Pts',(3.87597566474129,-1.3411816227841,1.25527603224183));
#5011=CARTESIAN_POINT('Ctrl Pts',(3.84137301409758,-1.37578427342781,1.27377192701083));
#5012=CARTESIAN_POINT('Ctrl Pts',(3.82608176712229,-1.3977169855633,1.28316729552365));
#5013=CARTESIAN_POINT('Ctrl Pts',(3.80537554685969,-1.44679575263487,1.29633569102376));
#5014=CARTESIAN_POINT('Ctrl Pts',(3.8,-1.47398753300333,1.3));
#5015=CARTESIAN_POINT('Ctrl Pts',(3.8,-1.5,1.3));
#5016=CARTESIAN_POINT('Origin',(4.,0.,0.9));
#5017=CARTESIAN_POINT('',(4.,-0.2,1.22360679774998));
#5018=CARTESIAN_POINT('',(4.2,-4.49191417939584E-18,1.3));
#5019=CARTESIAN_POINT('Ctrl Pts',(4.,-0.2,1.22360679774998));
#5020=CARTESIAN_POINT('Ctrl Pts',(4.02630182346442,-0.2,1.22360679774998));
#5021=CARTESIAN_POINT('Ctrl Pts',(4.05333179602069,-0.194568877616075,1.22872056892082));
#5022=CARTESIAN_POINT('Ctrl Pts',(4.10213335089966,-0.173983137835284,1.24474475389314));
#5023=CARTESIAN_POINT('Ctrl Pts',(4.12402433525871,-0.158818377215904,1.25527603224183));
#5024=CARTESIAN_POINT('Ctrl Pts',(4.15862698590242,-0.124215726572194,1.27377192701083));
#5025=CARTESIAN_POINT('Ctrl Pts',(4.17391823287771,-0.102283014436698,1.28316729552365));
#5026=CARTESIAN_POINT('Ctrl Pts',(4.19462445314031,-0.0532042473651346,
1.29633569102376));
#5027=CARTESIAN_POINT('Ctrl Pts',(4.2,-0.0260124669966693,1.3));
#5028=CARTESIAN_POINT('Ctrl Pts',(4.2,4.5102810375397E-17,1.3));
#5029=CARTESIAN_POINT('',(3.8,-6.08187253188241E-17,1.3));
#5030=CARTESIAN_POINT('Ctrl Pts',(3.8,-8.32667268468867E-17,1.3));
#5031=CARTESIAN_POINT('Ctrl Pts',(3.8,-0.0260124669966695,1.3));
#5032=CARTESIAN_POINT('Ctrl Pts',(3.80537554685969,-0.0532042473651335,
1.29633569102376));
#5033=CARTESIAN_POINT('Ctrl Pts',(3.82608176712229,-0.102283014436697,1.28316729552365));
#5034=CARTESIAN_POINT('Ctrl Pts',(3.84137301409758,-0.124215726572194,1.27377192701083));
#5035=CARTESIAN_POINT('Ctrl Pts',(3.87597566474129,-0.158818377215904,1.25527603224183));
#5036=CARTESIAN_POINT('Ctrl Pts',(3.89786664910035,-0.173983137835284,1.24474475389314));
#5037=CARTESIAN_POINT('Ctrl Pts',(3.94666820397931,-0.194568877616075,1.22872056892082));
#5038=CARTESIAN_POINT('Ctrl Pts',(3.97369817653558,-0.2,1.22360679774998));
#5039=CARTESIAN_POINT('Ctrl Pts',(4.,-0.2,1.22360679774998));
#5040=CARTESIAN_POINT('',(3.8,2.44929359829471E-17,2.));
#5041=CARTESIAN_POINT('',(3.8,-2.44929359829471E-17,0.9));
#5042=CARTESIAN_POINT('Origin',(4.,0.,2.));
#5043=CARTESIAN_POINT('Ctrl Pts',(4.2,2.77555756156289E-17,1.3));
#5044=CARTESIAN_POINT('Ctrl Pts',(4.2,0.0260124669966694,1.3));
#5045=CARTESIAN_POINT('Ctrl Pts',(4.19462445314031,0.0532042473651346,1.29633569102376));
#5046=CARTESIAN_POINT('Ctrl Pts',(4.17391823287771,0.102283014436698,1.28316729552365));
#5047=CARTESIAN_POINT('Ctrl Pts',(4.15862698590242,0.124215726572194,1.27377192701083));
#5048=CARTESIAN_POINT('Ctrl Pts',(4.12402433525871,0.158818377215904,1.25527603224183));
#5049=CARTESIAN_POINT('Ctrl Pts',(4.10213335089966,0.173983137835284,1.24474475389314));
#5050=CARTESIAN_POINT('Ctrl Pts',(4.05333179602069,0.194568877616075,1.22872056892082));
#5051=CARTESIAN_POINT('Ctrl Pts',(4.02630182346442,0.2,1.22360679774998));
#5052=CARTESIAN_POINT('Ctrl Pts',(3.97369817653558,0.2,1.22360679774998));
#5053=CARTESIAN_POINT('Ctrl Pts',(3.94666820397931,0.194568877616075,1.22872056892082));
#5054=CARTESIAN_POINT('Ctrl Pts',(3.89786664910035,0.173983137835284,1.24474475389314));
#5055=CARTESIAN_POINT('Ctrl Pts',(3.87597566474129,0.158818377215904,1.25527603224183));
#5056=CARTESIAN_POINT('Ctrl Pts',(3.84137301409758,0.124215726572194,1.27377192701083));
#5057=CARTESIAN_POINT('Ctrl Pts',(3.82608176712229,0.102283014436697,1.28316729552365));
#5058=CARTESIAN_POINT('Ctrl Pts',(3.80537554685969,0.0532042473651339,1.29633569102376));
#5059=CARTESIAN_POINT('Ctrl Pts',(3.8,0.0260124669966693,1.3));
#5060=CARTESIAN_POINT('Ctrl Pts',(3.8,-4.16333634234434E-17,1.3));
#5061=CARTESIAN_POINT('Origin',(4.,1.5,0.9));
#5062=CARTESIAN_POINT('',(4.,1.3,1.22360679774998));
#5063=CARTESIAN_POINT('',(4.2,1.5,1.3));
#5064=CARTESIAN_POINT('Ctrl Pts',(4.,1.3,1.22360679774998));
#5065=CARTESIAN_POINT('Ctrl Pts',(4.02630182346442,1.3,1.22360679774998));
#5066=CARTESIAN_POINT('Ctrl Pts',(4.05333179602069,1.30543112238393,1.22872056892082));
#5067=CARTESIAN_POINT('Ctrl Pts',(4.10213335089966,1.32601686216472,1.24474475389314));
#5068=CARTESIAN_POINT('Ctrl Pts',(4.12402433525871,1.3411816227841,1.25527603224183));
#5069=CARTESIAN_POINT('Ctrl Pts',(4.15862698590242,1.37578427342781,1.27377192701083));
#5070=CARTESIAN_POINT('Ctrl Pts',(4.17391823287771,1.3977169855633,1.28316729552365));
#5071=CARTESIAN_POINT('Ctrl Pts',(4.19462445314031,1.44679575263487,1.29633569102376));
#5072=CARTESIAN_POINT('Ctrl Pts',(4.2,1.47398753300333,1.3));
#5073=CARTESIAN_POINT('Ctrl Pts',(4.2,1.5,1.3));
#5074=CARTESIAN_POINT('',(3.8,1.5,1.3));
#5075=CARTESIAN_POINT('Ctrl Pts',(3.8,1.5,1.3));
#5076=CARTESIAN_POINT('Ctrl Pts',(3.8,1.47398753300333,1.3));
#5077=CARTESIAN_POINT('Ctrl Pts',(3.80537554685969,1.44679575263487,1.29633569102376));
#5078=CARTESIAN_POINT('Ctrl Pts',(3.82608176712229,1.3977169855633,1.28316729552365));
#5079=CARTESIAN_POINT('Ctrl Pts',(3.84137301409757,1.37578427342781,1.27377192701083));
#5080=CARTESIAN_POINT('Ctrl Pts',(3.87597566474129,1.3411816227841,1.25527603224183));
#5081=CARTESIAN_POINT('Ctrl Pts',(3.89786664910035,1.32601686216472,1.24474475389314));
#5082=CARTESIAN_POINT('Ctrl Pts',(3.94666820397931,1.30543112238393,1.22872056892082));
#5083=CARTESIAN_POINT('Ctrl Pts',(3.97369817653558,1.3,1.22360679774998));
#5084=CARTESIAN_POINT('Ctrl Pts',(4.,1.3,1.22360679774998));
#5085=CARTESIAN_POINT('',(3.8,1.5,2.));
#5086=CARTESIAN_POINT('',(3.8,1.5,0.9));
#5087=CARTESIAN_POINT('Origin',(4.,1.5,2.));
#5088=CARTESIAN_POINT('Ctrl Pts',(4.2,1.5,1.3));
#5089=CARTESIAN_POINT('Ctrl Pts',(4.2,1.52601246699667,1.3));
#5090=CARTESIAN_POINT('Ctrl Pts',(4.19462445314031,1.55320424736513,1.29633569102376));
#5091=CARTESIAN_POINT('Ctrl Pts',(4.17391823287771,1.6022830144367,1.28316729552365));
#5092=CARTESIAN_POINT('Ctrl Pts',(4.15862698590242,1.62421572657219,1.27377192701083));
#5093=CARTESIAN_POINT('Ctrl Pts',(4.12402433525871,1.6588183772159,1.25527603224183));
#5094=CARTESIAN_POINT('Ctrl Pts',(4.10213335089966,1.67398313783528,1.24474475389314));
#5095=CARTESIAN_POINT('Ctrl Pts',(4.05333179602069,1.69456887761607,1.22872056892082));
#5096=CARTESIAN_POINT('Ctrl Pts',(4.02630182346442,1.7,1.22360679774998));
#5097=CARTESIAN_POINT('Ctrl Pts',(3.97369817653558,1.7,1.22360679774998));
#5098=CARTESIAN_POINT('Ctrl Pts',(3.94666820397931,1.69456887761607,1.22872056892082));
#5099=CARTESIAN_POINT('Ctrl Pts',(3.89786664910035,1.67398313783528,1.24474475389314));
#5100=CARTESIAN_POINT('Ctrl Pts',(3.87597566474129,1.6588183772159,1.25527603224183));
#5101=CARTESIAN_POINT('Ctrl Pts',(3.84137301409758,1.62421572657219,1.27377192701083));
#5102=CARTESIAN_POINT('Ctrl Pts',(3.82608176712229,1.6022830144367,1.28316729552365));
#5103=CARTESIAN_POINT('Ctrl Pts',(3.80537554685969,1.55320424736513,1.29633569102376));
#5104=CARTESIAN_POINT('Ctrl Pts',(3.8,1.52601246699667,1.3));
#5105=CARTESIAN_POINT('Ctrl Pts',(3.8,1.5,1.3));
#5106=CARTESIAN_POINT('Origin',(-2.3,-2.4,0.8));
#5107=CARTESIAN_POINT('',(-2.465,-2.4,0.8));
#5108=CARTESIAN_POINT('Origin',(-2.3,-2.4,0.8));
#5109=CARTESIAN_POINT('',(-2.465,-2.4,2.));
#5110=CARTESIAN_POINT('',(-2.465,-2.4,0.8));
#5111=CARTESIAN_POINT('Origin',(-2.3,-2.4,2.));
#5112=CARTESIAN_POINT('Origin',(-2.3,-2.4,0.8));
#5113=CARTESIAN_POINT('Origin',(-5.7,2.4,0.8));
#5114=CARTESIAN_POINT('',(-5.865,2.4,0.8));
#5115=CARTESIAN_POINT('Origin',(-5.7,2.4,0.8));
#5116=CARTESIAN_POINT('',(-5.865,2.4,2.));
#5117=CARTESIAN_POINT('',(-5.865,2.4,0.8));
#5118=CARTESIAN_POINT('Origin',(-5.7,2.4,2.));
#5119=CARTESIAN_POINT('Origin',(-5.7,2.4,0.8));
#5120=CARTESIAN_POINT('Origin',(-5.7,-2.4,0.8));
#5121=CARTESIAN_POINT('',(-5.865,-2.4,0.8));
#5122=CARTESIAN_POINT('Origin',(-5.7,-2.4,0.8));
#5123=CARTESIAN_POINT('',(-5.865,-2.4,2.));
#5124=CARTESIAN_POINT('',(-5.865,-2.4,0.8));
#5125=CARTESIAN_POINT('Origin',(-5.7,-2.4,2.));
#5126=CARTESIAN_POINT('Origin',(-5.7,-2.4,0.8));
#5127=CARTESIAN_POINT('Origin',(-2.3,2.4,0.8));
#5128=CARTESIAN_POINT('',(-2.465,2.4,0.8));
#5129=CARTESIAN_POINT('Origin',(-2.3,2.4,0.8));
#5130=CARTESIAN_POINT('',(-2.465,2.4,2.));
#5131=CARTESIAN_POINT('',(-2.465,2.4,0.8));
#5132=CARTESIAN_POINT('Origin',(-2.3,2.4,2.));
#5133=CARTESIAN_POINT('Origin',(-2.3,2.4,0.8));
#5134=CARTESIAN_POINT('Origin',(-4.,-1.5,0.9));
#5135=CARTESIAN_POINT('',(-4.,-1.7,1.22360679774998));
#5136=CARTESIAN_POINT('',(-3.8,-1.5,1.3));
#5137=CARTESIAN_POINT('Ctrl Pts',(-4.,-1.7,1.22360679774998));
#5138=CARTESIAN_POINT('Ctrl Pts',(-3.97369817653558,-1.7,1.22360679774998));
#5139=CARTESIAN_POINT('Ctrl Pts',(-3.94666820397931,-1.69456887761608,1.22872056892082));
#5140=CARTESIAN_POINT('Ctrl Pts',(-3.89786664910035,-1.67398313783528,1.24474475389314));
#5141=CARTESIAN_POINT('Ctrl Pts',(-3.87597566474129,-1.6588183772159,1.25527603224183));
#5142=CARTESIAN_POINT('Ctrl Pts',(-3.84137301409758,-1.62421572657219,1.27377192701083));
#5143=CARTESIAN_POINT('Ctrl Pts',(-3.82608176712229,-1.6022830144367,1.28316729552365));
#5144=CARTESIAN_POINT('Ctrl Pts',(-3.80537554685969,-1.55320424736513,1.29633569102376));
#5145=CARTESIAN_POINT('Ctrl Pts',(-3.8,-1.52601246699667,1.3));
#5146=CARTESIAN_POINT('Ctrl Pts',(-3.8,-1.5,1.3));
#5147=CARTESIAN_POINT('',(-4.2,-1.5,1.3));
#5148=CARTESIAN_POINT('Ctrl Pts',(-4.2,-1.5,1.3));
#5149=CARTESIAN_POINT('Ctrl Pts',(-4.2,-1.52601246699667,1.3));
#5150=CARTESIAN_POINT('Ctrl Pts',(-4.19462445314031,-1.55320424736513,1.29633569102376));
#5151=CARTESIAN_POINT('Ctrl Pts',(-4.17391823287771,-1.6022830144367,1.28316729552365));
#5152=CARTESIAN_POINT('Ctrl Pts',(-4.15862698590242,-1.62421572657219,1.27377192701083));
#5153=CARTESIAN_POINT('Ctrl Pts',(-4.12402433525871,-1.6588183772159,1.25527603224183));
#5154=CARTESIAN_POINT('Ctrl Pts',(-4.10213335089965,-1.67398313783528,1.24474475389314));
#5155=CARTESIAN_POINT('Ctrl Pts',(-4.05333179602069,-1.69456887761608,1.22872056892082));
#5156=CARTESIAN_POINT('Ctrl Pts',(-4.02630182346442,-1.7,1.22360679774998));
#5157=CARTESIAN_POINT('Ctrl Pts',(-4.,-1.7,1.22360679774998));
#5158=CARTESIAN_POINT('',(-4.2,-1.5,2.));
#5159=CARTESIAN_POINT('',(-4.2,-1.5,0.9));
#5160=CARTESIAN_POINT('Origin',(-4.,-1.5,2.));
#5161=CARTESIAN_POINT('Ctrl Pts',(-3.8,-1.5,1.3));
#5162=CARTESIAN_POINT('Ctrl Pts',(-3.8,-1.47398753300333,1.3));
#5163=CARTESIAN_POINT('Ctrl Pts',(-3.80537554685969,-1.44679575263487,1.29633569102376));
#5164=CARTESIAN_POINT('Ctrl Pts',(-3.82608176712229,-1.3977169855633,1.28316729552365));
#5165=CARTESIAN_POINT('Ctrl Pts',(-3.84137301409758,-1.37578427342781,1.27377192701083));
#5166=CARTESIAN_POINT('Ctrl Pts',(-3.87597566474129,-1.3411816227841,1.25527603224183));
#5167=CARTESIAN_POINT('Ctrl Pts',(-3.89786664910035,-1.32601686216472,1.24474475389314));
#5168=CARTESIAN_POINT('Ctrl Pts',(-3.94666820397931,-1.30543112238392,1.22872056892082));
#5169=CARTESIAN_POINT('Ctrl Pts',(-3.97369817653558,-1.3,1.22360679774998));
#5170=CARTESIAN_POINT('Ctrl Pts',(-4.02630182346442,-1.3,1.22360679774998));
#5171=CARTESIAN_POINT('Ctrl Pts',(-4.05333179602069,-1.30543112238393,1.22872056892082));
#5172=CARTESIAN_POINT('Ctrl Pts',(-4.10213335089966,-1.32601686216472,1.24474475389314));
#5173=CARTESIAN_POINT('Ctrl Pts',(-4.12402433525871,-1.3411816227841,1.25527603224183));
#5174=CARTESIAN_POINT('Ctrl Pts',(-4.15862698590242,-1.37578427342781,1.27377192701083));
#5175=CARTESIAN_POINT('Ctrl Pts',(-4.17391823287771,-1.3977169855633,1.28316729552365));
#5176=CARTESIAN_POINT('Ctrl Pts',(-4.19462445314031,-1.44679575263487,1.29633569102376));
#5177=CARTESIAN_POINT('Ctrl Pts',(-4.2,-1.47398753300333,1.3));
#5178=CARTESIAN_POINT('Ctrl Pts',(-4.2,-1.5,1.3));
#5179=CARTESIAN_POINT('Origin',(-4.,0.,0.9));
#5180=CARTESIAN_POINT('',(-4.,-0.2,1.22360679774998));
#5181=CARTESIAN_POINT('',(-3.8,9.38587362841861E-18,1.3));
#5182=CARTESIAN_POINT('Ctrl Pts',(-4.,-0.2,1.22360679774998));
#5183=CARTESIAN_POINT('Ctrl Pts',(-3.97369817653558,-0.2,1.22360679774998));
#5184=CARTESIAN_POINT('Ctrl Pts',(-3.94666820397931,-0.194568877616075,
1.22872056892082));
#5185=CARTESIAN_POINT('Ctrl Pts',(-3.89786664910035,-0.173983137835284,
1.24474475389314));
#5186=CARTESIAN_POINT('Ctrl Pts',(-3.87597566474129,-0.158818377215904,
1.25527603224183));
#5187=CARTESIAN_POINT('Ctrl Pts',(-3.84137301409758,-0.124215726572194,
1.27377192701083));
#5188=CARTESIAN_POINT('Ctrl Pts',(-3.82608176712229,-0.102283014436697,
1.28316729552365));
#5189=CARTESIAN_POINT('Ctrl Pts',(-3.80537554685969,-0.053204247365134,
1.29633569102376));
#5190=CARTESIAN_POINT('Ctrl Pts',(-3.8,-0.0260124669966693,1.3));
#5191=CARTESIAN_POINT('Ctrl Pts',(-3.8,5.55111512312578E-17,1.3));
#5192=CARTESIAN_POINT('',(-4.2,-2.26548088473344E-17,1.3));
#5193=CARTESIAN_POINT('Ctrl Pts',(-4.2,-3.12250225675825E-17,1.3));
#5194=CARTESIAN_POINT('Ctrl Pts',(-4.2,-0.0260124669966694,1.3));
#5195=CARTESIAN_POINT('Ctrl Pts',(-4.19462445314031,-0.0532042473651348,
1.29633569102376));
#5196=CARTESIAN_POINT('Ctrl Pts',(-4.17391823287771,-0.102283014436698,
1.28316729552365));
#5197=CARTESIAN_POINT('Ctrl Pts',(-4.15862698590242,-0.124215726572194,
1.27377192701083));
#5198=CARTESIAN_POINT('Ctrl Pts',(-4.12402433525871,-0.158818377215904,
1.25527603224183));
#5199=CARTESIAN_POINT('Ctrl Pts',(-4.10213335089965,-0.173983137835285,
1.24474475389314));
#5200=CARTESIAN_POINT('Ctrl Pts',(-4.05333179602069,-0.194568877616075,
1.22872056892082));
#5201=CARTESIAN_POINT('Ctrl Pts',(-4.02630182346442,-0.2,1.22360679774998));
#5202=CARTESIAN_POINT('Ctrl Pts',(-4.,-0.2,1.22360679774998));
#5203=CARTESIAN_POINT('',(-4.2,2.44929359829471E-17,2.));
#5204=CARTESIAN_POINT('',(-4.2,-2.44929359829471E-17,0.9));
#5205=CARTESIAN_POINT('Origin',(-4.,0.,2.));
#5206=CARTESIAN_POINT('Ctrl Pts',(-3.8,5.55111512312578E-17,1.3));
#5207=CARTESIAN_POINT('Ctrl Pts',(-3.8,0.0260124669966694,1.3));
#5208=CARTESIAN_POINT('Ctrl Pts',(-3.80537554685969,0.053204247365134,1.29633569102376));
#5209=CARTESIAN_POINT('Ctrl Pts',(-3.82608176712229,0.102283014436697,1.28316729552365));
#5210=CARTESIAN_POINT('Ctrl Pts',(-3.84137301409758,0.124215726572194,1.27377192701083));
#5211=CARTESIAN_POINT('Ctrl Pts',(-3.87597566474129,0.158818377215904,1.25527603224183));
#5212=CARTESIAN_POINT('Ctrl Pts',(-3.89786664910035,0.173983137835284,1.24474475389314));
#5213=CARTESIAN_POINT('Ctrl Pts',(-3.94666820397931,0.194568877616075,1.22872056892082));
#5214=CARTESIAN_POINT('Ctrl Pts',(-3.97369817653558,0.2,1.22360679774998));
#5215=CARTESIAN_POINT('Ctrl Pts',(-4.02630182346442,0.2,1.22360679774998));
#5216=CARTESIAN_POINT('Ctrl Pts',(-4.05333179602069,0.194568877616075,1.22872056892082));
#5217=CARTESIAN_POINT('Ctrl Pts',(-4.10213335089966,0.173983137835284,1.24474475389314));
#5218=CARTESIAN_POINT('Ctrl Pts',(-4.12402433525871,0.158818377215904,1.25527603224183));
#5219=CARTESIAN_POINT('Ctrl Pts',(-4.15862698590242,0.124215726572194,1.27377192701083));
#5220=CARTESIAN_POINT('Ctrl Pts',(-4.17391823287771,0.102283014436697,1.28316729552365));
#5221=CARTESIAN_POINT('Ctrl Pts',(-4.19462445314031,0.0532042473651342,
1.29633569102376));
#5222=CARTESIAN_POINT('Ctrl Pts',(-4.2,0.0260124669966694,1.3));
#5223=CARTESIAN_POINT('Ctrl Pts',(-4.2,3.46944695195361E-18,1.3));
#5224=CARTESIAN_POINT('Origin',(-4.,1.5,0.9));
#5225=CARTESIAN_POINT('',(-4.,1.3,1.22360679774998));
#5226=CARTESIAN_POINT('',(-3.8,1.5,1.3));
#5227=CARTESIAN_POINT('Ctrl Pts',(-4.,1.3,1.22360679774998));
#5228=CARTESIAN_POINT('Ctrl Pts',(-3.97369817653558,1.3,1.22360679774998));
#5229=CARTESIAN_POINT('Ctrl Pts',(-3.94666820397931,1.30543112238392,1.22872056892082));
#5230=CARTESIAN_POINT('Ctrl Pts',(-3.89786664910035,1.32601686216472,1.24474475389314));
#5231=CARTESIAN_POINT('Ctrl Pts',(-3.87597566474129,1.3411816227841,1.25527603224183));
#5232=CARTESIAN_POINT('Ctrl Pts',(-3.84137301409758,1.37578427342781,1.27377192701083));
#5233=CARTESIAN_POINT('Ctrl Pts',(-3.82608176712229,1.3977169855633,1.28316729552365));
#5234=CARTESIAN_POINT('Ctrl Pts',(-3.80537554685969,1.44679575263487,1.29633569102376));
#5235=CARTESIAN_POINT('Ctrl Pts',(-3.8,1.47398753300333,1.3));
#5236=CARTESIAN_POINT('Ctrl Pts',(-3.8,1.5,1.3));
#5237=CARTESIAN_POINT('',(-4.2,1.5,1.3));
#5238=CARTESIAN_POINT('Ctrl Pts',(-4.2,1.5,1.3));
#5239=CARTESIAN_POINT('Ctrl Pts',(-4.2,1.47398753300333,1.3));
#5240=CARTESIAN_POINT('Ctrl Pts',(-4.19462445314031,1.44679575263487,1.29633569102376));
#5241=CARTESIAN_POINT('Ctrl Pts',(-4.17391823287771,1.3977169855633,1.28316729552365));
#5242=CARTESIAN_POINT('Ctrl Pts',(-4.15862698590242,1.37578427342781,1.27377192701083));
#5243=CARTESIAN_POINT('Ctrl Pts',(-4.12402433525871,1.3411816227841,1.25527603224183));
#5244=CARTESIAN_POINT('Ctrl Pts',(-4.10213335089965,1.32601686216472,1.24474475389314));
#5245=CARTESIAN_POINT('Ctrl Pts',(-4.05333179602069,1.30543112238392,1.22872056892082));
#5246=CARTESIAN_POINT('Ctrl Pts',(-4.02630182346442,1.3,1.22360679774998));
#5247=CARTESIAN_POINT('Ctrl Pts',(-4.,1.3,1.22360679774998));
#5248=CARTESIAN_POINT('',(-4.2,1.5,2.));
#5249=CARTESIAN_POINT('',(-4.2,1.5,0.9));
#5250=CARTESIAN_POINT('Origin',(-4.,1.5,2.));
#5251=CARTESIAN_POINT('Ctrl Pts',(-3.8,1.5,1.3));
#5252=CARTESIAN_POINT('Ctrl Pts',(-3.8,1.52601246699667,1.3));
#5253=CARTESIAN_POINT('Ctrl Pts',(-3.80537554685969,1.55320424736513,1.29633569102376));
#5254=CARTESIAN_POINT('Ctrl Pts',(-3.82608176712229,1.6022830144367,1.28316729552365));
#5255=CARTESIAN_POINT('Ctrl Pts',(-3.84137301409758,1.62421572657219,1.27377192701083));
#5256=CARTESIAN_POINT('Ctrl Pts',(-3.87597566474129,1.6588183772159,1.25527603224183));
#5257=CARTESIAN_POINT('Ctrl Pts',(-3.89786664910035,1.67398313783528,1.24474475389314));
#5258=CARTESIAN_POINT('Ctrl Pts',(-3.94666820397931,1.69456887761608,1.22872056892082));
#5259=CARTESIAN_POINT('Ctrl Pts',(-3.97369817653558,1.7,1.22360679774998));
#5260=CARTESIAN_POINT('Ctrl Pts',(-4.02630182346442,1.7,1.22360679774998));
#5261=CARTESIAN_POINT('Ctrl Pts',(-4.05333179602069,1.69456887761607,1.22872056892082));
#5262=CARTESIAN_POINT('Ctrl Pts',(-4.10213335089966,1.67398313783528,1.24474475389314));
#5263=CARTESIAN_POINT('Ctrl Pts',(-4.12402433525871,1.6588183772159,1.25527603224183));
#5264=CARTESIAN_POINT('Ctrl Pts',(-4.15862698590242,1.62421572657219,1.27377192701083));
#5265=CARTESIAN_POINT('Ctrl Pts',(-4.17391823287771,1.6022830144367,1.28316729552365));
#5266=CARTESIAN_POINT('Ctrl Pts',(-4.19462445314031,1.55320424736513,1.29633569102376));
#5267=CARTESIAN_POINT('Ctrl Pts',(-4.2,1.52601246699667,1.3));
#5268=CARTESIAN_POINT('Ctrl Pts',(-4.2,1.5,1.3));
#5269=CARTESIAN_POINT('Origin',(7.,-3.2,-0.1));
#5270=CARTESIAN_POINT('',(6.67,-3.2,0.));
#5271=CARTESIAN_POINT('Origin',(7.,-3.2,0.));
#5272=CARTESIAN_POINT('',(6.67,-3.2,2.));
#5273=CARTESIAN_POINT('',(6.67,-3.2,-0.1));
#5274=CARTESIAN_POINT('Origin',(7.,-3.2,2.));
#5275=CARTESIAN_POINT('Origin',(-7.,3.2,-0.1));
#5276=CARTESIAN_POINT('',(-7.33,3.2,0.));
#5277=CARTESIAN_POINT('Origin',(-7.,3.2,0.));
#5278=CARTESIAN_POINT('',(-7.33,3.2,2.));
#5279=CARTESIAN_POINT('',(-7.33,3.2,-0.1));
#5280=CARTESIAN_POINT('Origin',(-7.,3.2,2.));
#5281=CARTESIAN_POINT('Origin',(-7.,-3.2,-0.1));
#5282=CARTESIAN_POINT('',(-7.33,-3.2,0.));
#5283=CARTESIAN_POINT('Origin',(-7.,-3.2,0.));
#5284=CARTESIAN_POINT('',(-7.33,-3.2,2.));
#5285=CARTESIAN_POINT('',(-7.33,-3.2,-0.1));
#5286=CARTESIAN_POINT('Origin',(-7.,-3.2,2.));
#5287=CARTESIAN_POINT('Origin',(7.,3.2,-0.1));
#5288=CARTESIAN_POINT('',(6.67,3.2,0.));
#5289=CARTESIAN_POINT('Origin',(7.,3.2,0.));
#5290=CARTESIAN_POINT('',(6.67,3.2,2.));
#5291=CARTESIAN_POINT('',(6.67,3.2,-0.1));
#5292=CARTESIAN_POINT('Origin',(7.,3.2,2.));
#5293=CARTESIAN_POINT('Origin',(6.6,-1.5,1.));
#5294=CARTESIAN_POINT('',(6.6,-1.5,1.685));
#5295=CARTESIAN_POINT('Origin',(6.6,-1.5,1.));
#5296=CARTESIAN_POINT('',(8.,-1.5,1.685));
#5297=CARTESIAN_POINT('',(6.6,-1.5,1.685));
#5298=CARTESIAN_POINT('Origin',(8.,-1.5,1.));
#5299=CARTESIAN_POINT('Origin',(6.6,-1.5,1.));
#5300=CARTESIAN_POINT('',(6.6,-1.5,1.3));
#5301=CARTESIAN_POINT('Origin',(6.6,-1.5,1.));
#5302=CARTESIAN_POINT('Origin',(6.6,0.,1.));
#5303=CARTESIAN_POINT('',(6.6,-8.38883057415937E-17,1.685));
#5304=CARTESIAN_POINT('Origin',(6.6,0.,1.));
#5305=CARTESIAN_POINT('',(8.,8.38883057415937E-17,1.685));
#5306=CARTESIAN_POINT('',(6.6,-8.38883057415937E-17,1.685));
#5307=CARTESIAN_POINT('Origin',(8.,0.,1.));
#5308=CARTESIAN_POINT('Origin',(6.6,0.,1.));
#5309=CARTESIAN_POINT('',(6.6,-3.67394039744206E-17,1.3));
#5310=CARTESIAN_POINT('Origin',(6.6,0.,1.));
#5311=CARTESIAN_POINT('Origin',(6.6,1.5,1.));
#5312=CARTESIAN_POINT('',(6.6,1.5,1.685));
#5313=CARTESIAN_POINT('Origin',(6.6,1.5,1.));
#5314=CARTESIAN_POINT('',(8.,1.5,1.685));
#5315=CARTESIAN_POINT('',(6.6,1.5,1.685));
#5316=CARTESIAN_POINT('Origin',(8.,1.5,1.));
#5317=CARTESIAN_POINT('Origin',(6.6,1.5,1.));
#5318=CARTESIAN_POINT('',(6.6,1.5,1.3));
#5319=CARTESIAN_POINT('Origin',(6.6,1.5,1.));
#5320=CARTESIAN_POINT('Origin',(-8.1,-1.5,1.));
#5321=CARTESIAN_POINT('',(-8.,-1.5,1.685));
#5322=CARTESIAN_POINT('Origin',(-8.,-1.5,1.));
#5323=CARTESIAN_POINT('',(-6.6,-1.5,1.685));
#5324=CARTESIAN_POINT('',(-8.1,-1.5,1.685));
#5325=CARTESIAN_POINT('Origin',(-6.6,-1.5,1.));
#5326=CARTESIAN_POINT('Origin',(-6.6,-1.5,1.));
#5327=CARTESIAN_POINT('',(-6.6,-1.5,1.3));
#5328=CARTESIAN_POINT('Origin',(-6.6,-1.5,1.));
#5329=CARTESIAN_POINT('Origin',(-8.1,0.,1.));
#5330=CARTESIAN_POINT('',(-8.,-8.38883057415937E-17,1.685));
#5331=CARTESIAN_POINT('Origin',(-8.,0.,1.));
#5332=CARTESIAN_POINT('',(-6.6,-8.38883057415937E-17,1.685));
#5333=CARTESIAN_POINT('',(-8.1,-8.38883057415937E-17,1.685));
#5334=CARTESIAN_POINT('Origin',(-6.6,0.,1.));
#5335=CARTESIAN_POINT('Origin',(-6.6,0.,1.));
#5336=CARTESIAN_POINT('',(-6.6,3.67394039744206E-17,1.3));
#5337=CARTESIAN_POINT('Origin',(-6.6,0.,1.));
#5338=CARTESIAN_POINT('Origin',(-8.1,1.5,1.));
#5339=CARTESIAN_POINT('',(-8.,1.5,1.685));
#5340=CARTESIAN_POINT('Origin',(-8.,1.5,1.));
#5341=CARTESIAN_POINT('',(-6.6,1.5,1.685));
#5342=CARTESIAN_POINT('',(-8.1,1.5,1.685));
#5343=CARTESIAN_POINT('Origin',(-6.6,1.5,1.));
#5344=CARTESIAN_POINT('Origin',(-6.6,1.5,1.));
#5345=CARTESIAN_POINT('',(-6.6,1.5,1.3));
#5346=CARTESIAN_POINT('Origin',(-6.6,1.5,1.));
#5347=CARTESIAN_POINT('Origin',(-8.1,-1.5,1.));
#5348=CARTESIAN_POINT('',(-8.1,-1.5,1.3));
#5349=CARTESIAN_POINT('',(-8.1,-1.5,1.3));
#5350=CARTESIAN_POINT('',(-8.1,-1.5,1.3));
#5351=CARTESIAN_POINT('Origin',(-8.1,0.,1.));
#5352=CARTESIAN_POINT('',(-8.1,-3.67394039744206E-17,1.3));
#5353=CARTESIAN_POINT('',(-8.1,-3.67394039744206E-17,1.3));
#5354=CARTESIAN_POINT('',(-8.1,-3.67394039744206E-17,1.3));
#5355=CARTESIAN_POINT('Origin',(-8.1,1.5,1.));
#5356=CARTESIAN_POINT('',(-8.1,1.5,1.3));
#5357=CARTESIAN_POINT('',(-8.1,1.5,1.3));
#5358=CARTESIAN_POINT('',(-8.1,1.5,1.3));
#5359=CARTESIAN_POINT('Origin',(8.,4.,0.));
#5360=CARTESIAN_POINT('',(8.,4.,0.));
#5361=CARTESIAN_POINT('',(-8.,4.,0.));
#5362=CARTESIAN_POINT('',(8.,4.,0.));
#5363=CARTESIAN_POINT('',(-8.,4.,2.));
#5364=CARTESIAN_POINT('',(-8.,4.,0.));
#5365=CARTESIAN_POINT('',(8.,4.,2.));
#5366=CARTESIAN_POINT('',(8.,4.,2.));
#5367=CARTESIAN_POINT('',(8.,4.,0.));
#5368=CARTESIAN_POINT('Origin',(8.,-4.,0.));
#5369=CARTESIAN_POINT('',(8.,-4.,0.));
#5370=CARTESIAN_POINT('',(8.,-4.,0.));
#5371=CARTESIAN_POINT('',(8.,-4.,2.));
#5372=CARTESIAN_POINT('',(8.,-4.,2.));
#5373=CARTESIAN_POINT('',(8.,-4.,0.));
#5374=CARTESIAN_POINT('Origin',(-8.,-4.,0.));
#5375=CARTESIAN_POINT('',(-8.,-4.,0.));
#5376=CARTESIAN_POINT('',(-8.,-4.,0.));
#5377=CARTESIAN_POINT('',(-8.,-4.,2.));
#5378=CARTESIAN_POINT('',(-8.,-4.,2.));
#5379=CARTESIAN_POINT('',(-8.,-4.,0.));
#5380=CARTESIAN_POINT('Origin',(-8.,4.,0.));
#5381=CARTESIAN_POINT('',(-8.,4.,0.));
#5382=CARTESIAN_POINT('',(-8.,4.,2.));
#5383=CARTESIAN_POINT('Origin',(0.,0.,2.));
#5384=CARTESIAN_POINT('Origin',(0.,0.,0.));
#5385=CARTESIAN_POINT('',(0.,0.,0.));
#5386=CARTESIAN_POINT('Origin',(10.6,-1.6,0.826794919243112));
#5387=CARTESIAN_POINT('',(10.7,-1.6,0.876794919243112));
#5388=CARTESIAN_POINT('Origin',(10.7,-1.6,0.826794919243112));
#5389=CARTESIAN_POINT('',(11.1,-1.6,0.876794919243112));
#5390=CARTESIAN_POINT('',(10.6,-1.6,0.876794919243112));
#5391=CARTESIAN_POINT('Origin',(11.1,-1.6,0.826794919243112));
#5392=CARTESIAN_POINT('Origin',(10.6,-1.3,1.));
#5393=CARTESIAN_POINT('',(10.7,-1.3,1.05));
#5394=CARTESIAN_POINT('Origin',(10.7,-1.3,1.));
#5395=CARTESIAN_POINT('',(11.1,-1.3,1.05));
#5396=CARTESIAN_POINT('',(10.6,-1.3,1.05));
#5397=CARTESIAN_POINT('Origin',(11.1,-1.3,1.));
#5398=CARTESIAN_POINT('Origin',(10.6,-1.4,1.17320508075689));
#5399=CARTESIAN_POINT('',(10.7,-1.4,1.22320508075689));
#5400=CARTESIAN_POINT('Origin',(10.7,-1.4,1.17320508075689));
#5401=CARTESIAN_POINT('',(11.1,-1.4,1.22320508075689));
#5402=CARTESIAN_POINT('',(10.6,-1.4,1.22320508075689));
#5403=CARTESIAN_POINT('Origin',(11.1,-1.4,1.17320508075689));
#5404=CARTESIAN_POINT('Origin',(10.6,-1.6,1.17320508075689));
#5405=CARTESIAN_POINT('',(10.7,-1.6,1.22320508075689));
#5406=CARTESIAN_POINT('Origin',(10.7,-1.6,1.17320508075689));
#5407=CARTESIAN_POINT('',(11.1,-1.6,1.22320508075689));
#5408=CARTESIAN_POINT('',(10.6,-1.6,1.22320508075689));
#5409=CARTESIAN_POINT('Origin',(11.1,-1.6,1.17320508075689));
#5410=CARTESIAN_POINT('Origin',(10.6,-1.7,1.));
#5411=CARTESIAN_POINT('',(10.7,-1.7,1.05));
#5412=CARTESIAN_POINT('Origin',(10.7,-1.7,1.));
#5413=CARTESIAN_POINT('',(11.1,-1.7,1.05));
#5414=CARTESIAN_POINT('',(10.6,-1.7,1.05));
#5415=CARTESIAN_POINT('Origin',(11.1,-1.7,1.));
#5416=CARTESIAN_POINT('Origin',(10.6,-1.4,0.826794919243112));
#5417=CARTESIAN_POINT('',(10.7,-1.4,0.876794919243112));
#5418=CARTESIAN_POINT('Origin',(10.7,-1.4,0.826794919243112));
#5419=CARTESIAN_POINT('',(11.1,-1.4,0.876794919243112));
#5420=CARTESIAN_POINT('',(10.6,-1.4,0.876794919243112));
#5421=CARTESIAN_POINT('Origin',(11.1,-1.4,0.826794919243112));
#5422=CARTESIAN_POINT('Origin',(10.7,-1.5,1.));
#5423=CARTESIAN_POINT('',(10.7,-1.5,1.3));
#5424=CARTESIAN_POINT('Origin',(10.7,-1.5,1.));
#5425=CARTESIAN_POINT('Origin',(8.6,-1.5,1.));
#5426=CARTESIAN_POINT('',(8.6,-1.5,1.9));
#5427=CARTESIAN_POINT('Origin',(8.6,-1.5,1.));
#5428=CARTESIAN_POINT('',(8.6,-1.5,1.45));
#5429=CARTESIAN_POINT('Origin',(8.6,-1.5,1.));
#5430=CARTESIAN_POINT('Origin',(8.6,-1.5,1.));
#5431=CARTESIAN_POINT('',(11.1,-1.5,1.9));
#5432=CARTESIAN_POINT('Origin',(11.1,-1.5,1.));
#5433=CARTESIAN_POINT('',(8.6,-1.5,1.9));
#5434=CARTESIAN_POINT('Origin',(11.1,-1.5,1.));
#5435=CARTESIAN_POINT('Origin',(8.,-1.5,1.));
#5436=CARTESIAN_POINT('',(8.,-1.5,1.45));
#5437=CARTESIAN_POINT('',(8.,-1.5,1.45));
#5438=CARTESIAN_POINT('Origin',(8.,-1.5,1.));
#5439=CARTESIAN_POINT('Origin',(6.6,-1.5,1.));
#5440=CARTESIAN_POINT('',(6.6,-1.5,1.3));
#5441=CARTESIAN_POINT('',(6.6,-1.5,1.3));
#5442=CARTESIAN_POINT('Origin',(6.6,-1.5,1.));
#5443=CARTESIAN_POINT('Origin',(6.6,-1.5,1.));
#5444=CARTESIAN_POINT('',(8.,-1.5,1.685));
#5445=CARTESIAN_POINT('Origin',(8.,-1.5,1.));
#5446=CARTESIAN_POINT('',(6.6,-1.5,1.685));
#5447=CARTESIAN_POINT('',(6.6,-1.5,1.685));
#5448=CARTESIAN_POINT('Origin',(6.6,-1.5,1.));
#5449=CARTESIAN_POINT('Origin',(8.,-1.5,1.));
#5450=CARTESIAN_POINT('Origin',(6.6,-1.5,1.));
#5451=CARTESIAN_POINT('',(0.,0.,0.));
#5452=CARTESIAN_POINT('Origin',(10.6,1.4,0.826794919243112));
#5453=CARTESIAN_POINT('',(10.7,1.4,0.876794919243112));
#5454=CARTESIAN_POINT('Origin',(10.7,1.4,0.826794919243112));
#5455=CARTESIAN_POINT('',(11.1,1.4,0.876794919243112));
#5456=CARTESIAN_POINT('',(10.6,1.4,0.876794919243112));
#5457=CARTESIAN_POINT('Origin',(11.1,1.4,0.826794919243112));
#5458=CARTESIAN_POINT('Origin',(10.6,1.7,1.));
#5459=CARTESIAN_POINT('',(10.7,1.7,1.05));
#5460=CARTESIAN_POINT('Origin',(10.7,1.7,1.));
#5461=CARTESIAN_POINT('',(11.1,1.7,1.05));
#5462=CARTESIAN_POINT('',(10.6,1.7,1.05));
#5463=CARTESIAN_POINT('Origin',(11.1,1.7,1.));
#5464=CARTESIAN_POINT('Origin',(10.6,1.6,1.17320508075689));
#5465=CARTESIAN_POINT('',(10.7,1.6,1.22320508075689));
#5466=CARTESIAN_POINT('Origin',(10.7,1.6,1.17320508075689));
#5467=CARTESIAN_POINT('',(11.1,1.6,1.22320508075689));
#5468=CARTESIAN_POINT('',(10.6,1.6,1.22320508075689));
#5469=CARTESIAN_POINT('Origin',(11.1,1.6,1.17320508075689));
#5470=CARTESIAN_POINT('Origin',(10.6,1.4,1.17320508075689));
#5471=CARTESIAN_POINT('',(10.7,1.4,1.22320508075689));
#5472=CARTESIAN_POINT('Origin',(10.7,1.4,1.17320508075689));
#5473=CARTESIAN_POINT('',(11.1,1.4,1.22320508075689));
#5474=CARTESIAN_POINT('',(10.6,1.4,1.22320508075689));
#5475=CARTESIAN_POINT('Origin',(11.1,1.4,1.17320508075689));
#5476=CARTESIAN_POINT('Origin',(10.6,1.3,1.));
#5477=CARTESIAN_POINT('',(10.7,1.3,1.05));
#5478=CARTESIAN_POINT('Origin',(10.7,1.3,1.));
#5479=CARTESIAN_POINT('',(11.1,1.3,1.05));
#5480=CARTESIAN_POINT('',(10.6,1.3,1.05));
#5481=CARTESIAN_POINT('Origin',(11.1,1.3,1.));
#5482=CARTESIAN_POINT('Origin',(10.6,1.6,0.826794919243112));
#5483=CARTESIAN_POINT('',(10.7,1.6,0.876794919243112));
#5484=CARTESIAN_POINT('Origin',(10.7,1.6,0.826794919243112));
#5485=CARTESIAN_POINT('',(11.1,1.6,0.876794919243112));
#5486=CARTESIAN_POINT('',(10.6,1.6,0.876794919243112));
#5487=CARTESIAN_POINT('Origin',(11.1,1.6,0.826794919243112));
#5488=CARTESIAN_POINT('Origin',(10.7,1.5,1.));
#5489=CARTESIAN_POINT('',(10.7,1.5,1.3));
#5490=CARTESIAN_POINT('Origin',(10.7,1.5,1.));
#5491=CARTESIAN_POINT('Origin',(8.6,1.5,1.));
#5492=CARTESIAN_POINT('',(8.6,1.5,1.9));
#5493=CARTESIAN_POINT('Origin',(8.6,1.5,1.));
#5494=CARTESIAN_POINT('',(8.6,1.5,1.45));
#5495=CARTESIAN_POINT('Origin',(8.6,1.5,1.));
#5496=CARTESIAN_POINT('Origin',(8.6,1.5,1.));
#5497=CARTESIAN_POINT('',(11.1,1.5,1.9));
#5498=CARTESIAN_POINT('Origin',(11.1,1.5,1.));
#5499=CARTESIAN_POINT('',(8.6,1.5,1.9));
#5500=CARTESIAN_POINT('Origin',(11.1,1.5,1.));
#5501=CARTESIAN_POINT('Origin',(8.,1.5,1.));
#5502=CARTESIAN_POINT('',(8.,1.5,1.45));
#5503=CARTESIAN_POINT('',(8.,1.5,1.45));
#5504=CARTESIAN_POINT('Origin',(8.,1.5,1.));
#5505=CARTESIAN_POINT('Origin',(6.6,1.5,1.));
#5506=CARTESIAN_POINT('',(6.6,1.5,1.3));
#5507=CARTESIAN_POINT('',(6.6,1.5,1.3));
#5508=CARTESIAN_POINT('Origin',(6.6,1.5,1.));
#5509=CARTESIAN_POINT('Origin',(6.6,1.5,1.));
#5510=CARTESIAN_POINT('',(8.,1.5,1.685));
#5511=CARTESIAN_POINT('Origin',(8.,1.5,1.));
#5512=CARTESIAN_POINT('',(6.6,1.5,1.685));
#5513=CARTESIAN_POINT('',(6.6,1.5,1.685));
#5514=CARTESIAN_POINT('Origin',(6.6,1.5,1.));
#5515=CARTESIAN_POINT('Origin',(8.,1.5,1.));
#5516=CARTESIAN_POINT('Origin',(6.6,1.5,1.));
#5517=CARTESIAN_POINT('',(0.,0.,0.));
#5518=CARTESIAN_POINT('Origin',(0.,-0.4,0.));
#5519=CARTESIAN_POINT('',(1.01036297108185,-0.4,0.));
#5520=CARTESIAN_POINT('',(0.505181485540923,-0.4,0.875));
#5521=CARTESIAN_POINT('',(0.505181485540923,-0.4,0.875));
#5522=CARTESIAN_POINT('',(-0.505181485540923,-0.4,0.875));
#5523=CARTESIAN_POINT('',(-0.505181485540923,-0.4,0.875));
#5524=CARTESIAN_POINT('',(-1.01036297108185,-0.4,-1.23733777851239E-16));
#5525=CARTESIAN_POINT('',(-1.01036297108185,-0.4,-1.23733777851239E-16));
#5526=CARTESIAN_POINT('',(-0.505181485540922,-0.4,-0.875));
#5527=CARTESIAN_POINT('',(-0.505181485540922,-0.4,-0.875));
#5528=CARTESIAN_POINT('',(0.505181485540923,-0.4,-0.875));
#5529=CARTESIAN_POINT('',(0.505181485540923,-0.4,-0.875));
#5530=CARTESIAN_POINT('',(1.01036297108185,-0.4,0.));
#5531=CARTESIAN_POINT('',(-0.685,-0.4,-8.38883057415937E-17));
#5532=CARTESIAN_POINT('Origin',(0.,-0.4,0.));
#5533=CARTESIAN_POINT('Origin',(0.,0.4,0.));
#5534=CARTESIAN_POINT('',(0.505181485540923,0.4,0.875));
#5535=CARTESIAN_POINT('',(1.01036297108185,0.4,0.));
#5536=CARTESIAN_POINT('',(0.505181485540923,0.4,0.875));
#5537=CARTESIAN_POINT('',(0.505181485540923,0.4,-0.875));
#5538=CARTESIAN_POINT('',(1.01036297108185,0.4,0.));
#5539=CARTESIAN_POINT('',(-0.505181485540922,0.4,-0.875));
#5540=CARTESIAN_POINT('',(0.505181485540923,0.4,-0.875));
#5541=CARTESIAN_POINT('',(-1.01036297108185,0.4,-1.23733777851239E-16));
#5542=CARTESIAN_POINT('',(-0.505181485540922,0.4,-0.875));
#5543=CARTESIAN_POINT('',(-0.505181485540923,0.4,0.875));
#5544=CARTESIAN_POINT('',(-1.01036297108185,0.4,-1.23733777851239E-16));
#5545=CARTESIAN_POINT('',(-0.505181485540923,0.4,0.875));
#5546=CARTESIAN_POINT('',(-0.685,0.4,8.38883057415937E-17));
#5547=CARTESIAN_POINT('Origin',(0.,0.4,0.));
#5548=CARTESIAN_POINT('Origin',(-0.505181485540923,0.,0.875));
#5549=CARTESIAN_POINT('',(0.505181485540923,0.,0.875));
#5550=CARTESIAN_POINT('',(-0.505181485540923,0.,0.875));
#5551=CARTESIAN_POINT('Origin',(-1.01036297108185,0.,-1.23733777851239E-16));
#5552=CARTESIAN_POINT('',(-1.01036297108185,0.,-1.23733777851239E-16));
#5553=CARTESIAN_POINT('Origin',(-0.505181485540922,0.,-0.875));
#5554=CARTESIAN_POINT('',(-0.505181485540922,0.,-0.875));
#5555=CARTESIAN_POINT('Origin',(0.505181485540923,0.,-0.875));
#5556=CARTESIAN_POINT('',(0.505181485540923,0.,-0.875));
#5557=CARTESIAN_POINT('Origin',(1.01036297108185,0.,0.));
#5558=CARTESIAN_POINT('',(1.01036297108185,0.,0.));
#5559=CARTESIAN_POINT('Origin',(0.505181485540923,0.,0.875));
#5560=CARTESIAN_POINT('Origin',(0.,0.,0.));
#5561=CARTESIAN_POINT('',(-0.685,1.82,-8.38883057415937E-17));
#5562=CARTESIAN_POINT('',(-0.685,0.,-8.38883057415937E-17));
#5563=CARTESIAN_POINT('Origin',(0.,1.82,0.));
#5564=CARTESIAN_POINT('Origin',(0.605,1.9,0.));
#5565=CARTESIAN_POINT('',(-0.605,1.9,-7.40911313484149E-17));
#5566=CARTESIAN_POINT('Origin',(0.,1.9,0.));
#5567=CARTESIAN_POINT('',(-0.46,1.9,-5.63337527607782E-17));
#5568=CARTESIAN_POINT('Origin',(0.,1.9,0.));
#5569=CARTESIAN_POINT('Origin',(0.,1.86,0.));
#5570=CARTESIAN_POINT('',(-0.645,1.86,-7.89897185450043E-17));
#5571=CARTESIAN_POINT('Origin',(0.,0.,0.));
#5572=CARTESIAN_POINT('',(-0.685,-1.82,-8.38883057415937E-17));
#5573=CARTESIAN_POINT('Origin',(0.,-1.82,0.));
#5574=CARTESIAN_POINT('',(-0.685,0.,-8.38883057415937E-17));
#5575=CARTESIAN_POINT('Origin',(0.,-1.86,0.));
#5576=CARTESIAN_POINT('',(-0.605,-1.9,-7.40911313484149E-17));
#5577=CARTESIAN_POINT('Origin',(0.,-1.9,0.));
#5578=CARTESIAN_POINT('',(-0.645,-1.86,-7.89897185450043E-17));
#5579=CARTESIAN_POINT('Origin',(0.46,-1.9,0.));
#5580=CARTESIAN_POINT('',(-0.46,-1.9,-5.63337527607782E-17));
#5581=CARTESIAN_POINT('Origin',(0.,-1.9,0.));
#5582=CARTESIAN_POINT('Origin',(0.,0.,0.));
#5583=CARTESIAN_POINT('',(-0.46,0.,-5.63337527607782E-17));
#5584=CARTESIAN_POINT('',(0.,0.,0.));
#5585=CARTESIAN_POINT('Origin',(5.5,0.,3.5));
#5586=CARTESIAN_POINT('',(5.5,0.505181485540923,2.625));
#5587=CARTESIAN_POINT('',(5.5,1.01036297108185,3.5));
#5588=CARTESIAN_POINT('',(5.5,0.505181485540923,2.625));
#5589=CARTESIAN_POINT('',(5.5,-0.505181485540923,2.625));
#5590=CARTESIAN_POINT('',(5.5,-0.505181485540923,2.625));
#5591=CARTESIAN_POINT('',(5.5,-1.01036297108185,3.5));
#5592=CARTESIAN_POINT('',(5.5,-1.01036297108185,3.5));
#5593=CARTESIAN_POINT('',(5.5,-0.505181485540922,4.375));
#5594=CARTESIAN_POINT('',(5.5,-0.505181485540922,4.375));
#5595=CARTESIAN_POINT('',(5.5,0.505181485540923,4.375));
#5596=CARTESIAN_POINT('',(5.5,0.505181485540923,4.375));
#5597=CARTESIAN_POINT('',(5.5,1.01036297108185,3.5));
#5598=CARTESIAN_POINT('',(5.5,-8.38883057415937E-17,4.185));
#5599=CARTESIAN_POINT('Origin',(5.5,0.,3.5));
#5600=CARTESIAN_POINT('Origin',(5.5,-0.505181485540923,2.625));
#5601=CARTESIAN_POINT('',(6.1,0.505181485540923,2.625));
#5602=CARTESIAN_POINT('',(5.5,0.505181485540923,2.625));
#5603=CARTESIAN_POINT('',(6.1,-0.505181485540923,2.625));
#5604=CARTESIAN_POINT('',(6.1,-0.505181485540923,2.625));
#5605=CARTESIAN_POINT('',(5.5,-0.505181485540923,2.625));
#5606=CARTESIAN_POINT('Origin',(5.5,-1.01036297108185,3.5));
#5607=CARTESIAN_POINT('',(6.1,-1.01036297108185,3.5));
#5608=CARTESIAN_POINT('',(6.1,-1.01036297108185,3.5));
#5609=CARTESIAN_POINT('',(5.5,-1.01036297108185,3.5));
#5610=CARTESIAN_POINT('Origin',(5.5,-0.505181485540922,4.375));
#5611=CARTESIAN_POINT('',(6.1,-0.505181485540922,4.375));
#5612=CARTESIAN_POINT('',(6.1,-0.505181485540922,4.375));
#5613=CARTESIAN_POINT('',(5.5,-0.505181485540922,4.375));
#5614=CARTESIAN_POINT('Origin',(5.5,0.505181485540923,4.375));
#5615=CARTESIAN_POINT('',(6.1,0.505181485540923,4.375));
#5616=CARTESIAN_POINT('',(6.1,0.505181485540923,4.375));
#5617=CARTESIAN_POINT('',(5.5,0.505181485540923,4.375));
#5618=CARTESIAN_POINT('Origin',(5.5,1.01036297108185,3.5));
#5619=CARTESIAN_POINT('',(6.1,1.01036297108185,3.5));
#5620=CARTESIAN_POINT('',(6.1,1.01036297108185,3.5));
#5621=CARTESIAN_POINT('',(5.5,1.01036297108185,3.5));
#5622=CARTESIAN_POINT('Origin',(5.5,0.505181485540923,2.625));
#5623=CARTESIAN_POINT('',(6.1,0.505181485540923,2.625));
#5624=CARTESIAN_POINT('Origin',(6.1,0.,3.5));
#5625=CARTESIAN_POINT('Origin',(4.1,0.,3.5));
#5626=CARTESIAN_POINT('',(4.1,-8.38883057415937E-17,4.185));
#5627=CARTESIAN_POINT('',(4.1,-8.38883057415937E-17,4.185));
#5628=CARTESIAN_POINT('Origin',(4.1,0.,3.5));
#5629=CARTESIAN_POINT('Origin',(4.1,0.,3.5));
#5630=CARTESIAN_POINT('',(0.,0.,0.));
#5631=CARTESIAN_POINT('Origin',(5.3,-0.4,3.4));
#5632=CARTESIAN_POINT('',(5.5,0.4,3.4));
#5633=CARTESIAN_POINT('',(5.5,-0.4,3.4));
#5634=CARTESIAN_POINT('',(5.5,-0.2,3.4));
#5635=CARTESIAN_POINT('',(5.3,0.4,3.4));
#5636=CARTESIAN_POINT('',(5.3,0.4,3.4));
#5637=CARTESIAN_POINT('',(5.3,-0.4,3.4));
#5638=CARTESIAN_POINT('',(5.3,-0.4,3.4));
#5639=CARTESIAN_POINT('',(5.3,-0.4,3.4));
#5640=CARTESIAN_POINT('Origin',(5.3,-0.4,3.6));
#5641=CARTESIAN_POINT('',(5.5,-0.4,3.6));
#5642=CARTESIAN_POINT('',(5.5,-0.4,3.55));
#5643=CARTESIAN_POINT('',(5.3,-0.4,3.6));
#5644=CARTESIAN_POINT('',(5.3,-0.4,3.6));
#5645=CARTESIAN_POINT('',(5.3,-0.4,3.6));
#5646=CARTESIAN_POINT('Origin',(5.3,0.4,3.6));
#5647=CARTESIAN_POINT('',(5.5,0.4,3.6));
#5648=CARTESIAN_POINT('',(5.5,0.2,3.6));
#5649=CARTESIAN_POINT('',(5.3,0.4,3.6));
#5650=CARTESIAN_POINT('',(5.3,0.4,3.6));
#5651=CARTESIAN_POINT('',(5.3,0.4,3.6));
#5652=CARTESIAN_POINT('Origin',(5.3,0.4,3.4));
#5653=CARTESIAN_POINT('',(5.5,0.4,3.45));
#5654=CARTESIAN_POINT('',(5.3,0.4,3.4));
#5655=CARTESIAN_POINT('Origin',(5.3,0.,3.5));
#5656=CARTESIAN_POINT('Origin',(5.5,0.,3.5));
#5657=CARTESIAN_POINT('',(5.5,-8.38883057415937E-17,4.185));
#5658=CARTESIAN_POINT('Origin',(5.5,0.,3.5));
#5659=CARTESIAN_POINT('Origin',(4.1,0.,3.5));
#5660=CARTESIAN_POINT('',(4.1,-8.38883057415937E-17,4.185));
#5661=CARTESIAN_POINT('',(4.1,-8.38883057415937E-17,4.185));
#5662=CARTESIAN_POINT('Origin',(4.1,0.,3.5));
#5663=CARTESIAN_POINT('Origin',(4.1,0.,3.5));
#5664=CARTESIAN_POINT('',(0.,0.,0.));
#5665=CARTESIAN_POINT('',(0.,0.,0.));
#5666=CARTESIAN_POINT('Origin',(-2.3,-2.4,3.));
#5667=CARTESIAN_POINT('',(-2.7,-2.4,3.));
#5668=CARTESIAN_POINT('Origin',(-2.3,-2.4,3.));
#5669=CARTESIAN_POINT('',(-2.7,-2.4,5.2));
#5670=CARTESIAN_POINT('',(-2.7,-2.4,3.));
#5671=CARTESIAN_POINT('Origin',(-2.3,-2.4,5.2));
#5672=CARTESIAN_POINT('Origin',(-2.3,-2.4,3.));
#5673=CARTESIAN_POINT('',(-2.525,-2.4,3.));
#5674=CARTESIAN_POINT('Origin',(-2.3,-2.4,3.));
#5675=CARTESIAN_POINT('Origin',(-5.7,2.4,3.));
#5676=CARTESIAN_POINT('',(-6.1,2.4,3.));
#5677=CARTESIAN_POINT('Origin',(-5.7,2.4,3.));
#5678=CARTESIAN_POINT('',(-6.1,2.4,5.2));
#5679=CARTESIAN_POINT('',(-6.1,2.4,3.));
#5680=CARTESIAN_POINT('Origin',(-5.7,2.4,5.2));
#5681=CARTESIAN_POINT('Origin',(-5.7,2.4,3.));
#5682=CARTESIAN_POINT('',(-5.925,2.4,3.));
#5683=CARTESIAN_POINT('Origin',(-5.7,2.4,3.));
#5684=CARTESIAN_POINT('Origin',(-5.7,-2.4,3.));
#5685=CARTESIAN_POINT('',(-6.1,-2.4,3.));
#5686=CARTESIAN_POINT('Origin',(-5.7,-2.4,3.));
#5687=CARTESIAN_POINT('',(-6.1,-2.4,5.2));
#5688=CARTESIAN_POINT('',(-6.1,-2.4,3.));
#5689=CARTESIAN_POINT('Origin',(-5.7,-2.4,5.2));
#5690=CARTESIAN_POINT('Origin',(-5.7,-2.4,3.));
#5691=CARTESIAN_POINT('',(-5.925,-2.4,3.));
#5692=CARTESIAN_POINT('Origin',(-5.7,-2.4,3.));
#5693=CARTESIAN_POINT('Origin',(-2.3,2.4,3.));
#5694=CARTESIAN_POINT('',(-2.7,2.4,3.));
#5695=CARTESIAN_POINT('Origin',(-2.3,2.4,3.));
#5696=CARTESIAN_POINT('',(-2.7,2.4,5.2));
#5697=CARTESIAN_POINT('',(-2.7,2.4,3.));
#5698=CARTESIAN_POINT('Origin',(-2.3,2.4,5.2));
#5699=CARTESIAN_POINT('Origin',(-2.3,2.4,3.));
#5700=CARTESIAN_POINT('',(-2.525,2.4,3.));
#5701=CARTESIAN_POINT('Origin',(-2.3,2.4,3.));
#5702=CARTESIAN_POINT('Origin',(-2.3,-2.4,2.1));
#5703=CARTESIAN_POINT('',(-2.525,-2.4,2.2));
#5704=CARTESIAN_POINT('Origin',(-2.3,-2.4,2.2));
#5705=CARTESIAN_POINT('',(-2.525,-2.4,2.1));
#5706=CARTESIAN_POINT('Origin',(-5.7,2.4,2.1));
#5707=CARTESIAN_POINT('',(-5.925,2.4,2.2));
#5708=CARTESIAN_POINT('Origin',(-5.7,2.4,2.2));
#5709=CARTESIAN_POINT('',(-5.925,2.4,2.1));
#5710=CARTESIAN_POINT('Origin',(-5.7,-2.4,2.1));
#5711=CARTESIAN_POINT('',(-5.925,-2.4,2.2));
#5712=CARTESIAN_POINT('Origin',(-5.7,-2.4,2.2));
#5713=CARTESIAN_POINT('',(-5.925,-2.4,2.1));
#5714=CARTESIAN_POINT('Origin',(-2.3,2.4,2.1));
#5715=CARTESIAN_POINT('',(-2.525,2.4,2.2));
#5716=CARTESIAN_POINT('Origin',(-2.3,2.4,2.2));
#5717=CARTESIAN_POINT('',(-2.525,2.4,2.1));
#5718=CARTESIAN_POINT('Origin',(-4.,0.,4.));
#5719=CARTESIAN_POINT('',(-4.685,-8.38883057415937E-17,4.));
#5720=CARTESIAN_POINT('Origin',(-4.,0.,4.));
#5721=CARTESIAN_POINT('',(-4.685,8.38883057415937E-17,5.2));
#5722=CARTESIAN_POINT('',(-4.685,-8.38883057415937E-17,4.));
#5723=CARTESIAN_POINT('Origin',(-4.,0.,5.2));
#5724=CARTESIAN_POINT('Origin',(-4.,0.,4.));
#5725=CARTESIAN_POINT('',(-4.2,-2.44929359829471E-17,4.));
#5726=CARTESIAN_POINT('Origin',(-4.,0.,4.));
#5727=CARTESIAN_POINT('Origin',(-4.,-1.5,2.1));
#5728=CARTESIAN_POINT('',(-4.2,-1.5,2.2));
#5729=CARTESIAN_POINT('Origin',(-4.,-1.5,2.2));
#5730=CARTESIAN_POINT('',(-4.2,-1.5,5.2));
#5731=CARTESIAN_POINT('',(-4.2,-1.5,2.1));
#5732=CARTESIAN_POINT('Origin',(-4.,-1.5,5.2));
#5733=CARTESIAN_POINT('Origin',(-4.,0.,2.1));
#5734=CARTESIAN_POINT('',(-4.2,-2.44929359829471E-17,2.2));
#5735=CARTESIAN_POINT('Origin',(-4.,0.,2.2));
#5736=CARTESIAN_POINT('',(-4.2,-2.44929359829471E-17,2.1));
#5737=CARTESIAN_POINT('Origin',(-4.,1.5,2.1));
#5738=CARTESIAN_POINT('',(-4.2,1.5,2.2));
#5739=CARTESIAN_POINT('Origin',(-4.,1.5,2.2));
#5740=CARTESIAN_POINT('',(-4.2,1.5,5.2));
#5741=CARTESIAN_POINT('',(-4.2,1.5,2.1));
#5742=CARTESIAN_POINT('Origin',(-4.,1.5,5.2));
#5743=CARTESIAN_POINT('Origin',(-1.5,3.,2.2));
#5744=CARTESIAN_POINT('',(-1.5,3.,2.2));
#5745=CARTESIAN_POINT('',(-6.5,3.,2.2));
#5746=CARTESIAN_POINT('',(-1.5,3.,2.2));
#5747=CARTESIAN_POINT('',(-6.5,3.,5.2));
#5748=CARTESIAN_POINT('',(-6.5,3.,2.2));
#5749=CARTESIAN_POINT('',(-1.5,3.,5.2));
#5750=CARTESIAN_POINT('',(-1.5,3.,5.2));
#5751=CARTESIAN_POINT('',(-1.5,3.,2.2));
#5752=CARTESIAN_POINT('Origin',(-1.5,-3.,2.2));
#5753=CARTESIAN_POINT('',(-1.5,-3.,2.2));
#5754=CARTESIAN_POINT('',(-1.5,-3.,2.2));
#5755=CARTESIAN_POINT('',(-1.5,-3.,5.2));
#5756=CARTESIAN_POINT('',(-1.5,-3.,5.2));
#5757=CARTESIAN_POINT('',(-1.5,-3.,2.2));
#5758=CARTESIAN_POINT('Origin',(-6.5,-3.,2.2));
#5759=CARTESIAN_POINT('',(-6.5,-3.,2.2));
#5760=CARTESIAN_POINT('',(-6.5,-3.,2.2));
#5761=CARTESIAN_POINT('',(-6.5,-3.,5.2));
#5762=CARTESIAN_POINT('',(-6.5,-3.,5.2));
#5763=CARTESIAN_POINT('',(-6.5,-3.,2.2));
#5764=CARTESIAN_POINT('Origin',(-6.5,3.,2.2));
#5765=CARTESIAN_POINT('',(-6.5,3.,2.2));
#5766=CARTESIAN_POINT('',(-6.5,3.,5.2));
#5767=CARTESIAN_POINT('Origin',(-4.,0.,5.2));
#5768=CARTESIAN_POINT('Origin',(-4.,0.,2.2));
#5769=CARTESIAN_POINT('',(0.,0.,0.));
#5770=CARTESIAN_POINT('Origin',(-2.3,-2.4,1.9));
#5771=CARTESIAN_POINT('',(-2.525,-2.4,2.));
#5772=CARTESIAN_POINT('Origin',(-2.3,-2.4,2.));
#5773=CARTESIAN_POINT('',(-2.525,-2.4,2.2));
#5774=CARTESIAN_POINT('',(-2.525,-2.4,1.9));
#5775=CARTESIAN_POINT('Origin',(-2.3,-2.4,2.2));
#5776=CARTESIAN_POINT('Origin',(-5.7,2.4,1.9));
#5777=CARTESIAN_POINT('',(-5.925,2.4,2.));
#5778=CARTESIAN_POINT('Origin',(-5.7,2.4,2.));
#5779=CARTESIAN_POINT('',(-5.925,2.4,2.2));
#5780=CARTESIAN_POINT('',(-5.925,2.4,1.9));
#5781=CARTESIAN_POINT('Origin',(-5.7,2.4,2.2));
#5782=CARTESIAN_POINT('Origin',(-5.7,-2.4,1.9));
#5783=CARTESIAN_POINT('',(-5.925,-2.4,2.));
#5784=CARTESIAN_POINT('Origin',(-5.7,-2.4,2.));
#5785=CARTESIAN_POINT('',(-5.925,-2.4,2.2));
#5786=CARTESIAN_POINT('',(-5.925,-2.4,1.9));
#5787=CARTESIAN_POINT('Origin',(-5.7,-2.4,2.2));
#5788=CARTESIAN_POINT('Origin',(-2.3,2.4,1.9));
#5789=CARTESIAN_POINT('',(-2.525,2.4,2.));
#5790=CARTESIAN_POINT('Origin',(-2.3,2.4,2.));
#5791=CARTESIAN_POINT('',(-2.525,2.4,2.2));
#5792=CARTESIAN_POINT('',(-2.525,2.4,1.9));
#5793=CARTESIAN_POINT('Origin',(-2.3,2.4,2.2));
#5794=CARTESIAN_POINT('Origin',(-4.,-1.5,1.9));
#5795=CARTESIAN_POINT('',(-4.2,-1.5,2.));
#5796=CARTESIAN_POINT('Origin',(-4.,-1.5,2.));
#5797=CARTESIAN_POINT('',(-4.2,-1.5,2.2));
#5798=CARTESIAN_POINT('',(-4.2,-1.5,1.9));
#5799=CARTESIAN_POINT('Origin',(-4.,-1.5,2.2));
#5800=CARTESIAN_POINT('Origin',(-4.,0.,1.9));
#5801=CARTESIAN_POINT('',(-4.2,-2.44929359829471E-17,2.));
#5802=CARTESIAN_POINT('Origin',(-4.,0.,2.));
#5803=CARTESIAN_POINT('',(-4.2,2.44929359829471E-17,2.2));
#5804=CARTESIAN_POINT('',(-4.2,-2.44929359829471E-17,1.9));
#5805=CARTESIAN_POINT('Origin',(-4.,0.,2.2));
#5806=CARTESIAN_POINT('Origin',(-4.,1.5,1.9));
#5807=CARTESIAN_POINT('',(-4.2,1.5,2.));
#5808=CARTESIAN_POINT('Origin',(-4.,1.5,2.));
#5809=CARTESIAN_POINT('',(-4.2,1.5,2.2));
#5810=CARTESIAN_POINT('',(-4.2,1.5,1.9));
#5811=CARTESIAN_POINT('Origin',(-4.,1.5,2.2));
#5812=CARTESIAN_POINT('Origin',(-1.5,3.,2.));
#5813=CARTESIAN_POINT('',(-1.5,3.,2.));
#5814=CARTESIAN_POINT('',(-6.5,3.,2.));
#5815=CARTESIAN_POINT('',(-1.5,3.,2.));
#5816=CARTESIAN_POINT('',(-6.5,3.,2.2));
#5817=CARTESIAN_POINT('',(-6.5,3.,2.));
#5818=CARTESIAN_POINT('',(-1.5,3.,2.2));
#5819=CARTESIAN_POINT('',(-1.5,3.,2.2));
#5820=CARTESIAN_POINT('',(-1.5,3.,2.));
#5821=CARTESIAN_POINT('Origin',(-1.5,-3.,2.));
#5822=CARTESIAN_POINT('',(-1.5,-3.,2.));
#5823=CARTESIAN_POINT('',(-1.5,-3.,2.));
#5824=CARTESIAN_POINT('',(-1.5,-3.,2.2));
#5825=CARTESIAN_POINT('',(-1.5,-3.,2.2));
#5826=CARTESIAN_POINT('',(-1.5,-3.,2.));
#5827=CARTESIAN_POINT('Origin',(-6.5,-3.,2.));
#5828=CARTESIAN_POINT('',(-6.5,-3.,2.));
#5829=CARTESIAN_POINT('',(-6.5,-3.,2.));
#5830=CARTESIAN_POINT('',(-6.5,-3.,2.2));
#5831=CARTESIAN_POINT('',(-6.5,-3.,2.2));
#5832=CARTESIAN_POINT('',(-6.5,-3.,2.));
#5833=CARTESIAN_POINT('Origin',(-6.5,3.,2.));
#5834=CARTESIAN_POINT('',(-6.5,3.,2.));
#5835=CARTESIAN_POINT('',(-6.5,3.,2.2));
#5836=CARTESIAN_POINT('Origin',(-4.,0.,2.2));
#5837=CARTESIAN_POINT('Origin',(-4.,0.,2.));
#5838=CARTESIAN_POINT('',(0.,0.,0.));
#5839=CARTESIAN_POINT('Origin',(-3.75,0.,4.85));
#5840=CARTESIAN_POINT('',(-4.265,-6.30693101560887E-17,4.85));
#5841=CARTESIAN_POINT('Origin',(-3.75,0.,4.85));
#5842=CARTESIAN_POINT('',(-4.265,6.30693101560887E-17,5.5));
#5843=CARTESIAN_POINT('',(-4.265,-6.30693101560887E-17,4.85));
#5844=CARTESIAN_POINT('Origin',(-3.75,0.,5.5));
#5845=CARTESIAN_POINT('Origin',(-3.75,0.,4.85));
#5846=CARTESIAN_POINT('',(-3.95,-2.44929359829471E-17,4.85));
#5847=CARTESIAN_POINT('Origin',(-3.75,0.,4.85));
#5848=CARTESIAN_POINT('Origin',(-3.75,0.,5.));
#5849=CARTESIAN_POINT('',(-3.24481851445908,-0.875,5.));
#5850=CARTESIAN_POINT('',(-2.73963702891815,0.,5.));
#5851=CARTESIAN_POINT('',(-3.24481851445908,-0.875,5.));
#5852=CARTESIAN_POINT('',(-4.25518148554092,-0.875,5.));
#5853=CARTESIAN_POINT('',(-4.25518148554092,-0.875,5.));
#5854=CARTESIAN_POINT('',(-4.76036297108184,1.23733777851239E-16,5.));
#5855=CARTESIAN_POINT('',(-4.76036297108184,1.23733777851239E-16,5.));
#5856=CARTESIAN_POINT('',(-4.25518148554092,0.875,5.));
#5857=CARTESIAN_POINT('',(-4.25518148554092,0.875,5.));
#5858=CARTESIAN_POINT('',(-3.24481851445908,0.875,5.));
#5859=CARTESIAN_POINT('',(-3.24481851445908,0.875,5.));
#5860=CARTESIAN_POINT('',(-2.73963702891815,0.,5.));
#5861=CARTESIAN_POINT('',(-4.435,-8.38883057415937E-17,5.));
#5862=CARTESIAN_POINT('Origin',(-3.75,0.,5.));
#5863=CARTESIAN_POINT('Origin',(-4.25518148554092,-0.875,5.));
#5864=CARTESIAN_POINT('',(-3.24481851445908,-0.875,5.5));
#5865=CARTESIAN_POINT('',(-3.24481851445908,-0.875,5.));
#5866=CARTESIAN_POINT('',(-4.25518148554092,-0.875,5.5));
#5867=CARTESIAN_POINT('',(-4.25518148554092,-0.875,5.5));
#5868=CARTESIAN_POINT('',(-4.25518148554092,-0.875,5.));
#5869=CARTESIAN_POINT('Origin',(-4.76036297108184,1.23733777851239E-16,
5.));
#5870=CARTESIAN_POINT('',(-4.76036297108184,1.11022302462516E-16,5.5));
#5871=CARTESIAN_POINT('',(-4.76036297108184,1.23733777851239E-16,5.5));
#5872=CARTESIAN_POINT('',(-4.76036297108184,1.23733777851239E-16,5.));
#5873=CARTESIAN_POINT('Origin',(-4.25518148554092,0.875,5.));
#5874=CARTESIAN_POINT('',(-4.25518148554092,0.875,5.5));
#5875=CARTESIAN_POINT('',(-4.25518148554092,0.875,5.5));
#5876=CARTESIAN_POINT('',(-4.25518148554092,0.875,5.));
#5877=CARTESIAN_POINT('Origin',(-3.24481851445908,0.875,5.));
#5878=CARTESIAN_POINT('',(-3.24481851445908,0.875,5.5));
#5879=CARTESIAN_POINT('',(-3.24481851445908,0.875,5.5));
#5880=CARTESIAN_POINT('',(-3.24481851445908,0.875,5.));
#5881=CARTESIAN_POINT('Origin',(-2.73963702891815,0.,5.));
#5882=CARTESIAN_POINT('',(-2.73963702891815,0.,5.5));
#5883=CARTESIAN_POINT('',(-2.73963702891815,0.,5.5));
#5884=CARTESIAN_POINT('',(-2.73963702891815,0.,5.));
#5885=CARTESIAN_POINT('Origin',(-3.24481851445908,-0.875,5.));
#5886=CARTESIAN_POINT('',(-3.24481851445908,-0.875,5.5));
#5887=CARTESIAN_POINT('Origin',(-3.75,0.,5.5));
#5888=CARTESIAN_POINT('Origin',(-3.75,0.,3.8));
#5889=CARTESIAN_POINT('',(-3.95,-2.44929359829471E-17,3.8));
#5890=CARTESIAN_POINT('',(-3.95,-2.44929359829471E-17,3.8));
#5891=CARTESIAN_POINT('Origin',(-3.75,0.,3.8));
#5892=CARTESIAN_POINT('Origin',(-3.75,0.,3.8));
#5893=CARTESIAN_POINT('',(-4.435,-8.38883057415937E-17,3.8));
#5894=CARTESIAN_POINT('',(-4.435,-8.38883057415937E-17,3.8));
#5895=CARTESIAN_POINT('Origin',(-3.75,0.,3.8));
#5896=CARTESIAN_POINT('Origin',(-3.75,0.,3.8));
#5897=CARTESIAN_POINT('',(0.,0.,0.));
#5898=CARTESIAN_POINT('',(0.,0.,0.));
#5899=CARTESIAN_POINT('Origin',(0.,0.6,0.));
#5900=CARTESIAN_POINT('',(-0.43,0.6,5.26598123633362E-17));
#5901=CARTESIAN_POINT('Origin',(0.,0.6,0.));
#5902=CARTESIAN_POINT('',(-0.43,0.7,-5.26598123633362E-17));
#5903=CARTESIAN_POINT('',(-0.43,0.6,5.26598123633362E-17));
#5904=CARTESIAN_POINT('Origin',(0.,0.7,0.));
#5905=CARTESIAN_POINT('Origin',(0.,0.6,0.));
#5906=CARTESIAN_POINT('',(-0.2,0.6,2.44929359829471E-17));
#5907=CARTESIAN_POINT('Origin',(0.,0.6,0.));
#5908=CARTESIAN_POINT('Origin',(0.,0.5,-1.11022302462516E-16));
#5909=CARTESIAN_POINT('',(0.346410161513776,0.5,0.6));
#5910=CARTESIAN_POINT('',(0.692820323027551,0.5,0.));
#5911=CARTESIAN_POINT('',(0.346410161513776,0.5,0.6));
#5912=CARTESIAN_POINT('',(0.346410161513776,0.5,-0.6));
#5913=CARTESIAN_POINT('',(0.692820323027551,0.5,0.));
#5914=CARTESIAN_POINT('',(-0.346410161513775,0.5,-0.6));
#5915=CARTESIAN_POINT('',(0.346410161513776,0.5,-0.6));
#5916=CARTESIAN_POINT('',(-0.692820323027551,0.5,-8.48460190979926E-17));
#5917=CARTESIAN_POINT('',(-0.346410161513775,0.5,-0.6));
#5918=CARTESIAN_POINT('',(-0.346410161513776,0.5,0.6));
#5919=CARTESIAN_POINT('',(-0.692820323027551,0.5,-8.48460190979926E-17));
#5920=CARTESIAN_POINT('',(-0.346410161513776,0.5,0.6));
#5921=CARTESIAN_POINT('',(-0.525,0.5,-6.4293956955236E-17));
#5922=CARTESIAN_POINT('Origin',(0.,0.5,0.));
#5923=CARTESIAN_POINT('Origin',(0.,0.,-1.11022302462516E-16));
#5924=CARTESIAN_POINT('',(0.346410161513776,0.,0.6));
#5925=CARTESIAN_POINT('',(0.692820323027551,0.,0.));
#5926=CARTESIAN_POINT('',(0.346410161513776,0.,0.6));
#5927=CARTESIAN_POINT('',(-0.346410161513776,0.,0.6));
#5928=CARTESIAN_POINT('',(-0.346410161513776,0.,0.6));
#5929=CARTESIAN_POINT('',(-0.692820323027551,0.,-8.48460190979926E-17));
#5930=CARTESIAN_POINT('',(-0.692820323027551,0.,-8.48460190979926E-17));
#5931=CARTESIAN_POINT('',(-0.346410161513775,0.,-0.6));
#5932=CARTESIAN_POINT('',(-0.346410161513775,0.,-0.6));
#5933=CARTESIAN_POINT('',(0.346410161513776,0.,-0.6));
#5934=CARTESIAN_POINT('',(0.346410161513776,0.,-0.6));
#5935=CARTESIAN_POINT('',(0.692820323027551,0.,0.));
#5936=CARTESIAN_POINT('',(-0.515,0.,-6.30693101560887E-17));
#5937=CARTESIAN_POINT('Origin',(0.,0.,0.));
#5938=CARTESIAN_POINT('Origin',(-0.346410161513776,0.,0.6));
#5939=CARTESIAN_POINT('',(0.346410161513776,0.,0.6));
#5940=CARTESIAN_POINT('',(-0.346410161513776,0.,0.6));
#5941=CARTESIAN_POINT('Origin',(-0.692820323027551,0.,-8.48460190979926E-17));
#5942=CARTESIAN_POINT('',(-0.692820323027551,0.,-8.48460190979926E-17));
#5943=CARTESIAN_POINT('Origin',(-0.346410161513775,0.,-0.6));
#5944=CARTESIAN_POINT('',(-0.346410161513775,0.,-0.6));
#5945=CARTESIAN_POINT('Origin',(0.346410161513776,0.,-0.6));
#5946=CARTESIAN_POINT('',(0.346410161513776,0.,-0.6));
#5947=CARTESIAN_POINT('Origin',(0.692820323027551,0.,0.));
#5948=CARTESIAN_POINT('',(0.692820323027551,0.,0.));
#5949=CARTESIAN_POINT('Origin',(0.346410161513776,0.,0.6));
#5950=CARTESIAN_POINT('Origin',(0.46,0.7,0.));
#5951=CARTESIAN_POINT('',(-0.46,0.7,-5.63337527607782E-17));
#5952=CARTESIAN_POINT('Origin',(0.,0.7,0.));
#5953=CARTESIAN_POINT('Origin',(0.,1.2,0.));
#5954=CARTESIAN_POINT('',(-0.46,1.7,-5.63337527607782E-17));
#5955=CARTESIAN_POINT('',(-0.46,1.2,-5.63337527607782E-17));
#5956=CARTESIAN_POINT('Origin',(0.,1.7,0.));
#5957=CARTESIAN_POINT('Origin',(0.525,1.7,0.));
#5958=CARTESIAN_POINT('',(-0.525,1.7,-6.4293956955236E-17));
#5959=CARTESIAN_POINT('Origin',(0.,1.7,0.));
#5960=CARTESIAN_POINT('Origin',(0.,1.1,0.));
#5961=CARTESIAN_POINT('',(-0.525,1.1,-6.4293956955236E-17));
#5962=CARTESIAN_POINT('Origin',(0.,-0.325,0.));
#5963=CARTESIAN_POINT('',(-0.515,-0.65,-6.30693101560887E-17));
#5964=CARTESIAN_POINT('Origin',(0.,-0.65,0.));
#5965=CARTESIAN_POINT('',(-0.515,-0.325,-6.30693101560887E-17));
#5966=CARTESIAN_POINT('Origin',(0.2,-0.65,0.));
#5967=CARTESIAN_POINT('',(-0.2,-0.65,-2.44929359829471E-17));
#5968=CARTESIAN_POINT('Origin',(0.,-0.65,0.));
#5969=CARTESIAN_POINT('Origin',(0.,0.0249999999999999,0.));
#5970=CARTESIAN_POINT('',(-0.2,0.0249999999999999,-2.44929359829471E-17));
#5971=CARTESIAN_POINT('',(0.,0.,0.));
#5972=CARTESIAN_POINT('Origin',(0.475,1.95,0.));
#5973=CARTESIAN_POINT('',(-0.475,1.95,-5.81707229594993E-17));
#5974=CARTESIAN_POINT('Origin',(0.,1.95,0.));
#5975=CARTESIAN_POINT('',(-0.31,1.95,-3.7964050773568E-17));
#5976=CARTESIAN_POINT('Origin',(0.,1.95,0.));
#5977=CARTESIAN_POINT('Origin',(0.,1.825,0.));
#5978=CARTESIAN_POINT('',(-0.475,1.7,-5.81707229594993E-17));
#5979=CARTESIAN_POINT('Origin',(0.,1.7,0.));
#5980=CARTESIAN_POINT('',(-0.475,1.825,-5.81707229594993E-17));
#5981=CARTESIAN_POINT('Origin',(0.355,1.7,0.));
#5982=CARTESIAN_POINT('',(-0.355,1.7,-4.3474961369731E-17));
#5983=CARTESIAN_POINT('Origin',(0.,1.7,0.));
#5984=CARTESIAN_POINT('Origin',(0.,1.55,0.));
#5985=CARTESIAN_POINT('',(-0.355,1.4,-4.3474961369731E-17));
#5986=CARTESIAN_POINT('Origin',(0.,1.4,0.));
#5987=CARTESIAN_POINT('',(-0.355,1.55,-4.3474961369731E-17));
#5988=CARTESIAN_POINT('Origin',(0.31,1.4,0.));
#5989=CARTESIAN_POINT('',(-0.31,1.4,-3.7964050773568E-17));
#5990=CARTESIAN_POINT('Origin',(0.,1.4,0.));
#5991=CARTESIAN_POINT('Origin',(0.,1.675,0.));
#5992=CARTESIAN_POINT('',(-0.31,1.675,-3.7964050773568E-17));
#5993=CARTESIAN_POINT('',(0.,0.,0.));
#5994=CARTESIAN_POINT('',(0.,0.,0.));
#5995=CARTESIAN_POINT('',(0.,0.,0.));
#5996=CARTESIAN_POINT('Origin',(0.3,0.4,0.));
#5997=CARTESIAN_POINT('',(-0.3,0.4,-3.67394039744206E-17));
#5998=CARTESIAN_POINT('Origin',(0.,0.4,0.));
#5999=CARTESIAN_POINT('Origin',(0.,0.375,0.));
#6000=CARTESIAN_POINT('',(-0.35,0.35,-4.28626379701573E-17));
#6001=CARTESIAN_POINT('Origin',(0.,0.35,0.));
#6002=CARTESIAN_POINT('',(-0.325,0.375,-3.9801020972289E-17));
#6003=CARTESIAN_POINT('Origin',(0.,0.19,0.));
#6004=CARTESIAN_POINT('',(-0.35,0.03,-4.28626379701574E-17));
#6005=CARTESIAN_POINT('Origin',(0.,0.03,0.));
#6006=CARTESIAN_POINT('',(-0.35,0.19,-4.28626379701574E-17));
#6007=CARTESIAN_POINT('Origin',(0.,0.0149999999999999,0.));
#6008=CARTESIAN_POINT('',(-0.32,-3.29597460435593E-17,-3.91886975727153E-17));
#6009=CARTESIAN_POINT('Origin',(0.,0.,0.));
#6010=CARTESIAN_POINT('',(-0.335,0.0149999999999999,-4.10256677714363E-17));
#6011=CARTESIAN_POINT('Origin',(0.22,0.,0.));
#6012=CARTESIAN_POINT('',(-0.22,-6.93889390390723E-18,-2.69422295812418E-17));
#6013=CARTESIAN_POINT('Origin',(0.,0.,0.));
#6014=CARTESIAN_POINT('Origin',(0.,-0.02,0.));
#6015=CARTESIAN_POINT('',(-0.1954,-0.0492,2.39295984553393E-17));
#6016=CARTESIAN_POINT('Origin',(0.,-0.0492,0.));
#6017=CARTESIAN_POINT('',(-0.21,-0.02,-2.57175827820944E-17));
#6018=CARTESIAN_POINT('Origin',(0.,-0.8,0.));
#6019=CARTESIAN_POINT('',(-0.1954,-1.5646,2.39295984553393E-17));
#6020=CARTESIAN_POINT('Origin',(0.,-1.5646,0.));
#6021=CARTESIAN_POINT('',(-0.1954,-0.8,-2.39295984553393E-17));
#6022=CARTESIAN_POINT('Origin',(0.,-1.58,0.));
#6023=CARTESIAN_POINT('',(-0.16,-1.6,-1.95943487863577E-17));
#6024=CARTESIAN_POINT('Origin',(0.,-1.6,0.));
#6025=CARTESIAN_POINT('',(-0.18,-1.58,-2.20436423846524E-17));
#6026=CARTESIAN_POINT('Origin',(0.,-1.6,0.));
#6027=CARTESIAN_POINT('Origin',(0.0866025403784439,-0.4,-0.15));
#6028=CARTESIAN_POINT('',(0.173205080756888,-0.4,0.));
#6029=CARTESIAN_POINT('',(0.0866025403784439,-0.4,-0.15));
#6030=CARTESIAN_POINT('',(0.173205080756888,-0.4,0.));
#6031=CARTESIAN_POINT('',(0.0866025403784439,-0.64,-0.15));
#6032=CARTESIAN_POINT('',(0.0866025403784439,-0.4,-0.15));
#6033=CARTESIAN_POINT('',(0.173205080756888,-0.64,0.));
#6034=CARTESIAN_POINT('',(0.173205080756888,-0.64,0.));
#6035=CARTESIAN_POINT('',(0.173205080756888,-0.4,0.));
#6036=CARTESIAN_POINT('Origin',(-0.0866025403784438,-0.4,-0.15));
#6037=CARTESIAN_POINT('',(-0.0866025403784438,-0.4,-0.15));
#6038=CARTESIAN_POINT('',(0.0866025403784439,-0.4,-0.15));
#6039=CARTESIAN_POINT('',(-0.0866025403784438,-0.64,-0.15));
#6040=CARTESIAN_POINT('',(-0.0866025403784438,-0.4,-0.15));
#6041=CARTESIAN_POINT('',(0.0866025403784439,-0.64,-0.15));
#6042=CARTESIAN_POINT('Origin',(-0.173205080756888,-0.4,-2.77555756156289E-17));
#6043=CARTESIAN_POINT('',(-0.173205080756888,-0.4,-2.12115047744981E-17));
#6044=CARTESIAN_POINT('',(-0.0866025403784438,-0.4,-0.15));
#6045=CARTESIAN_POINT('',(-0.173205080756888,-0.64,-2.77555756156289E-17));
#6046=CARTESIAN_POINT('',(-0.173205080756888,-0.4,-2.12115047744981E-17));
#6047=CARTESIAN_POINT('',(-0.0866025403784438,-0.64,-0.15));
#6048=CARTESIAN_POINT('Origin',(-0.0866025403784439,-0.4,0.15));
#6049=CARTESIAN_POINT('',(-0.0866025403784439,-0.4,0.15));
#6050=CARTESIAN_POINT('',(-0.173205080756888,-0.4,-2.12115047744981E-17));
#6051=CARTESIAN_POINT('',(-0.0866025403784439,-0.64,0.15));
#6052=CARTESIAN_POINT('',(-0.0866025403784439,-0.4,0.15));
#6053=CARTESIAN_POINT('',(-0.173205080756888,-0.64,-2.12115047744981E-17));
#6054=CARTESIAN_POINT('Origin',(0.0866025403784439,-0.4,0.15));
#6055=CARTESIAN_POINT('',(0.0866025403784439,-0.4,0.15));
#6056=CARTESIAN_POINT('',(-0.0866025403784439,-0.4,0.15));
#6057=CARTESIAN_POINT('',(0.0866025403784439,-0.64,0.15));
#6058=CARTESIAN_POINT('',(0.0866025403784439,-0.4,0.15));
#6059=CARTESIAN_POINT('',(-0.0866025403784439,-0.64,0.15));
#6060=CARTESIAN_POINT('Origin',(0.173205080756888,-0.4,0.));
#6061=CARTESIAN_POINT('',(0.0866025403784439,-0.4,0.15));
#6062=CARTESIAN_POINT('',(0.0866025403784439,-0.64,0.15));
#6063=CARTESIAN_POINT('Origin',(0.,-0.4,-2.77555756156289E-17));
#6064=CARTESIAN_POINT('Origin',(0.,-0.64,-2.77555756156289E-17));
#6065=CARTESIAN_POINT('',(0.,0.,0.));
#6066=CARTESIAN_POINT('',(0.,0.,0.));
#6067=CARTESIAN_POINT('',(-0.25,0.,0.2));
#6068=CARTESIAN_POINT('',(-4.,0.,5.7));
#6069=CARTESIAN_POINT('',(-5.7,-2.4,3.));
#6070=CARTESIAN_POINT('',(-2.3,2.4,3.));
#6071=CARTESIAN_POINT('',(-2.3,-2.4,3.));
#6072=CARTESIAN_POINT('',(-5.7,2.4,3.));
#6073=CARTESIAN_POINT('',(0.,0.,0.));
#6074=CARTESIAN_POINT('',(0.,0.,0.));
#6075=CARTESIAN_POINT('',(0.,0.,0.));
#6076=CARTESIAN_POINT('',(-8.5,0.,1.));
#6077=CARTESIAN_POINT('',(2.5,0.,-2.5));
#6078=CARTESIAN_POINT('',(-2.5,-1.5,-2.5));
#6079=CARTESIAN_POINT('',(-2.5,1.5,-2.5));
#6080=CARTESIAN_POINT('',(0.,0.,0.));
#6081=CARTESIAN_POINT('',(8.,-4.36742145716513E-15,2.66453525910038E-15));
#6082=UNCERTAINTY_MEASURE_WITH_UNIT(LENGTH_MEASURE(0.001),#6114,
'DISTANCE_ACCURACY_VALUE',
'Maximum model space distance between geometric entities at asserted c
onnectivities');
#6083=UNCERTAINTY_MEASURE_WITH_UNIT(LENGTH_MEASURE(0.001),#6114,
'DISTANCE_ACCURACY_VALUE',
'Maximum model space distance between geometric entities at asserted c
onnectivities');
#6084=UNCERTAINTY_MEASURE_WITH_UNIT(LENGTH_MEASURE(0.001),#6114,
'DISTANCE_ACCURACY_VALUE',
'Maximum model space distance between geometric entities at asserted c
onnectivities');
#6085=UNCERTAINTY_MEASURE_WITH_UNIT(LENGTH_MEASURE(0.001),#6114,
'DISTANCE_ACCURACY_VALUE',
'Maximum model space distance between geometric entities at asserted c
onnectivities');
#6086=UNCERTAINTY_MEASURE_WITH_UNIT(LENGTH_MEASURE(0.001),#6114,
'DISTANCE_ACCURACY_VALUE',
'Maximum model space distance between geometric entities at asserted c
onnectivities');
#6087=UNCERTAINTY_MEASURE_WITH_UNIT(LENGTH_MEASURE(0.001),#6114,
'DISTANCE_ACCURACY_VALUE',
'Maximum model space distance between geometric entities at asserted c
onnectivities');
#6088=UNCERTAINTY_MEASURE_WITH_UNIT(LENGTH_MEASURE(0.001),#6114,
'DISTANCE_ACCURACY_VALUE',
'Maximum model space distance between geometric entities at asserted c
onnectivities');
#6089=UNCERTAINTY_MEASURE_WITH_UNIT(LENGTH_MEASURE(0.001),#6114,
'DISTANCE_ACCURACY_VALUE',
'Maximum model space distance between geometric entities at asserted c
onnectivities');
#6090=UNCERTAINTY_MEASURE_WITH_UNIT(LENGTH_MEASURE(0.001),#6114,
'DISTANCE_ACCURACY_VALUE',
'Maximum model space distance between geometric entities at asserted c
onnectivities');
#6091=UNCERTAINTY_MEASURE_WITH_UNIT(LENGTH_MEASURE(0.001),#6114,
'DISTANCE_ACCURACY_VALUE',
'Maximum model space distance between geometric entities at asserted c
onnectivities');
#6092=UNCERTAINTY_MEASURE_WITH_UNIT(LENGTH_MEASURE(0.001),#6114,
'DISTANCE_ACCURACY_VALUE',
'Maximum model space distance between geometric entities at asserted c
onnectivities');
#6093=UNCERTAINTY_MEASURE_WITH_UNIT(LENGTH_MEASURE(0.001),#6114,
'DISTANCE_ACCURACY_VALUE',
'Maximum model space distance between geometric entities at asserted c
onnectivities');
#6094=UNCERTAINTY_MEASURE_WITH_UNIT(LENGTH_MEASURE(0.001),#6114,
'DISTANCE_ACCURACY_VALUE',
'Maximum model space distance between geometric entities at asserted c
onnectivities');
#6095=UNCERTAINTY_MEASURE_WITH_UNIT(LENGTH_MEASURE(0.001),#6114,
'DISTANCE_ACCURACY_VALUE',
'Maximum model space distance between geometric entities at asserted c
onnectivities');
#6096=UNCERTAINTY_MEASURE_WITH_UNIT(LENGTH_MEASURE(0.001),#6114,
'DISTANCE_ACCURACY_VALUE',
'Maximum model space distance between geometric entities at asserted c
onnectivities');
#6097=UNCERTAINTY_MEASURE_WITH_UNIT(LENGTH_MEASURE(0.001),#6114,
'DISTANCE_ACCURACY_VALUE',
'Maximum model space distance between geometric entities at asserted c
onnectivities');
#6098=(
GEOMETRIC_REPRESENTATION_CONTEXT(3)
GLOBAL_UNCERTAINTY_ASSIGNED_CONTEXT((#6082))
GLOBAL_UNIT_ASSIGNED_CONTEXT((#6114,#6116,#6117))
REPRESENTATION_CONTEXT('','3D')
);
#6099=(
GEOMETRIC_REPRESENTATION_CONTEXT(3)
GLOBAL_UNCERTAINTY_ASSIGNED_CONTEXT((#6083))
GLOBAL_UNIT_ASSIGNED_CONTEXT((#6114,#6116,#6117))
REPRESENTATION_CONTEXT('','3D')
);
#6100=(
GEOMETRIC_REPRESENTATION_CONTEXT(3)
GLOBAL_UNCERTAINTY_ASSIGNED_CONTEXT((#6084))
GLOBAL_UNIT_ASSIGNED_CONTEXT((#6114,#6116,#6117))
REPRESENTATION_CONTEXT('','3D')
);
#6101=(
GEOMETRIC_REPRESENTATION_CONTEXT(3)
GLOBAL_UNCERTAINTY_ASSIGNED_CONTEXT((#6085))
GLOBAL_UNIT_ASSIGNED_CONTEXT((#6114,#6116,#6117))
REPRESENTATION_CONTEXT('','3D')
);
#6102=(
GEOMETRIC_REPRESENTATION_CONTEXT(3)
GLOBAL_UNCERTAINTY_ASSIGNED_CONTEXT((#6086))
GLOBAL_UNIT_ASSIGNED_CONTEXT((#6114,#6116,#6117))
REPRESENTATION_CONTEXT('','3D')
);
#6103=(
GEOMETRIC_REPRESENTATION_CONTEXT(3)
GLOBAL_UNCERTAINTY_ASSIGNED_CONTEXT((#6087))
GLOBAL_UNIT_ASSIGNED_CONTEXT((#6114,#6116,#6117))
REPRESENTATION_CONTEXT('','3D')
);
#6104=(
GEOMETRIC_REPRESENTATION_CONTEXT(3)
GLOBAL_UNCERTAINTY_ASSIGNED_CONTEXT((#6088))
GLOBAL_UNIT_ASSIGNED_CONTEXT((#6114,#6116,#6117))
REPRESENTATION_CONTEXT('','3D')
);
#6105=(
GEOMETRIC_REPRESENTATION_CONTEXT(3)
GLOBAL_UNCERTAINTY_ASSIGNED_CONTEXT((#6089))
GLOBAL_UNIT_ASSIGNED_CONTEXT((#6114,#6116,#6117))
REPRESENTATION_CONTEXT('','3D')
);
#6106=(
GEOMETRIC_REPRESENTATION_CONTEXT(3)
GLOBAL_UNCERTAINTY_ASSIGNED_CONTEXT((#6090))
GLOBAL_UNIT_ASSIGNED_CONTEXT((#6114,#6116,#6117))
REPRESENTATION_CONTEXT('','3D')
);
#6107=(
GEOMETRIC_REPRESENTATION_CONTEXT(3)
GLOBAL_UNCERTAINTY_ASSIGNED_CONTEXT((#6091))
GLOBAL_UNIT_ASSIGNED_CONTEXT((#6114,#6116,#6117))
REPRESENTATION_CONTEXT('','3D')
);
#6108=(
GEOMETRIC_REPRESENTATION_CONTEXT(3)
GLOBAL_UNCERTAINTY_ASSIGNED_CONTEXT((#6092))
GLOBAL_UNIT_ASSIGNED_CONTEXT((#6114,#6116,#6117))
REPRESENTATION_CONTEXT('','3D')
);
#6109=(
GEOMETRIC_REPRESENTATION_CONTEXT(3)
GLOBAL_UNCERTAINTY_ASSIGNED_CONTEXT((#6093))
GLOBAL_UNIT_ASSIGNED_CONTEXT((#6114,#6116,#6117))
REPRESENTATION_CONTEXT('','3D')
);
#6110=(
GEOMETRIC_REPRESENTATION_CONTEXT(3)
GLOBAL_UNCERTAINTY_ASSIGNED_CONTEXT((#6094))
GLOBAL_UNIT_ASSIGNED_CONTEXT((#6114,#6116,#6117))
REPRESENTATION_CONTEXT('','3D')
);
#6111=(
GEOMETRIC_REPRESENTATION_CONTEXT(3)
GLOBAL_UNCERTAINTY_ASSIGNED_CONTEXT((#6095))
GLOBAL_UNIT_ASSIGNED_CONTEXT((#6114,#6116,#6117))
REPRESENTATION_CONTEXT('','3D')
);
#6112=(
GEOMETRIC_REPRESENTATION_CONTEXT(3)
GLOBAL_UNCERTAINTY_ASSIGNED_CONTEXT((#6096))
GLOBAL_UNIT_ASSIGNED_CONTEXT((#6114,#6116,#6117))
REPRESENTATION_CONTEXT('','3D')
);
#6113=(
GEOMETRIC_REPRESENTATION_CONTEXT(3)
GLOBAL_UNCERTAINTY_ASSIGNED_CONTEXT((#6097))
GLOBAL_UNIT_ASSIGNED_CONTEXT((#6114,#6116,#6117))
REPRESENTATION_CONTEXT('','3D')
);
#6114=(
LENGTH_UNIT()
NAMED_UNIT(*)
SI_UNIT(.CENTI.,.METRE.)
);
#6115=(
LENGTH_UNIT()
NAMED_UNIT(*)
SI_UNIT($,.METRE.)
);
#6116=(
NAMED_UNIT(*)
PLANE_ANGLE_UNIT()
SI_UNIT($,.RADIAN.)
);
#6117=(
NAMED_UNIT(*)
SI_UNIT($,.STERADIAN.)
SOLID_ANGLE_UNIT()
);
#6118=SHAPE_DEFINITION_REPRESENTATION(#6133,#6167);
#6119=SHAPE_DEFINITION_REPRESENTATION(#6134,#6168);
#6120=SHAPE_DEFINITION_REPRESENTATION(#6135,#6169);
#6121=SHAPE_DEFINITION_REPRESENTATION(#6136,#6170);
#6122=SHAPE_DEFINITION_REPRESENTATION(#6137,#6171);
#6123=SHAPE_DEFINITION_REPRESENTATION(#6138,#6172);
#6124=SHAPE_DEFINITION_REPRESENTATION(#6139,#6173);
#6125=SHAPE_DEFINITION_REPRESENTATION(#6140,#6174);
#6126=SHAPE_DEFINITION_REPRESENTATION(#6141,#6175);
#6127=SHAPE_DEFINITION_REPRESENTATION(#6142,#6176);
#6128=SHAPE_DEFINITION_REPRESENTATION(#6143,#6177);
#6129=SHAPE_DEFINITION_REPRESENTATION(#6144,#6178);
#6130=SHAPE_DEFINITION_REPRESENTATION(#6145,#6179);
#6131=SHAPE_DEFINITION_REPRESENTATION(#6146,#6180);
#6132=SHAPE_DEFINITION_REPRESENTATION(#6149,#6181);
#6133=PRODUCT_DEFINITION_SHAPE('',$,#6183);
#6134=PRODUCT_DEFINITION_SHAPE('',$,#6184);
#6135=PRODUCT_DEFINITION_SHAPE('',$,#6185);
#6136=PRODUCT_DEFINITION_SHAPE('',$,#6186);
#6137=PRODUCT_DEFINITION_SHAPE('',$,#6187);
#6138=PRODUCT_DEFINITION_SHAPE('',$,#6188);
#6139=PRODUCT_DEFINITION_SHAPE('',$,#6189);
#6140=PRODUCT_DEFINITION_SHAPE('',$,#6190);
#6141=PRODUCT_DEFINITION_SHAPE('',$,#6191);
#6142=PRODUCT_DEFINITION_SHAPE('',$,#6192);
#6143=PRODUCT_DEFINITION_SHAPE('',$,#6193);
#6144=PRODUCT_DEFINITION_SHAPE('',$,#6194);
#6145=PRODUCT_DEFINITION_SHAPE('',$,#6195);
#6146=PRODUCT_DEFINITION_SHAPE('',$,#6196);
#6147=PRODUCT_DEFINITION_SHAPE($,$,#70);
#6148=PRODUCT_DEFINITION_SHAPE($,$,#71);
#6149=PRODUCT_DEFINITION_SHAPE('',$,#6197);
#6150=PRODUCT_DEFINITION_SHAPE($,$,#72);
#6151=PRODUCT_DEFINITION_SHAPE($,$,#73);
#6152=PRODUCT_DEFINITION_SHAPE($,$,#74);
#6153=PRODUCT_DEFINITION_SHAPE($,$,#75);
#6154=PRODUCT_DEFINITION_SHAPE($,$,#76);
#6155=PRODUCT_DEFINITION_SHAPE($,$,#77);
#6156=PRODUCT_DEFINITION_SHAPE($,$,#78);
#6157=PRODUCT_DEFINITION_SHAPE($,$,#79);
#6158=PRODUCT_DEFINITION_SHAPE($,$,#80);
#6159=PRODUCT_DEFINITION_SHAPE($,$,#81);
#6160=PRODUCT_DEFINITION_SHAPE($,$,#82);
#6161=PRODUCT_DEFINITION_SHAPE($,$,#83);
#6162=PRODUCT_DEFINITION_SHAPE($,$,#84);
#6163=PRODUCT_DEFINITION_SHAPE($,$,#85);
#6164=PRODUCT_DEFINITION_SHAPE($,$,#86);
#6165=PRODUCT_DEFINITION_SHAPE($,$,#87);
#6166=PRODUCT_DEFINITION_SHAPE($,$,#88);
#6167=SHAPE_REPRESENTATION('',(#3504,#3896,#3897,#3898,#3899,#3900,#3901,
#3902,#3903,#3904),#6098);
#6168=SHAPE_REPRESENTATION('',(#3505),#6099);
#6169=SHAPE_REPRESENTATION('',(#3601),#6100);
#6170=SHAPE_REPRESENTATION('',(#3637),#6101);
#6171=SHAPE_REPRESENTATION('',(#3673),#6102);
#6172=SHAPE_REPRESENTATION('',(#3697),#6103);
#6173=SHAPE_REPRESENTATION('',(#3710),#6104);
#6174=SHAPE_REPRESENTATION('',(#3721,#3888,#3889,#3890,#3891,#3892,#3893,
#3894,#3895),#6105);
#6175=SHAPE_REPRESENTATION('',(#3722),#6106);
#6176=SHAPE_REPRESENTATION('',(#3770),#6107);
#6177=SHAPE_REPRESENTATION('',(#3798),#6108);
#6178=SHAPE_REPRESENTATION('',(#3818,#3860,#3861),#6109);
#6179=SHAPE_REPRESENTATION('',(#3819),#6110);
#6180=SHAPE_REPRESENTATION('',(#3847),#6111);
#6181=SHAPE_REPRESENTATION('',(#3862),#6112);
#6182=PRODUCT_DEFINITION_CONTEXT('part definition',#6229,'design');
#6183=PRODUCT_DEFINITION('PAT-108',
'PAT-108',#6198,#6182);
#6184=PRODUCT_DEFINITION('Valve sub-base','Valve sub-base',#6199,
#6182);
#6185=PRODUCT_DEFINITION('Exhaust silencer envelope',
'Exhaust silencer envelope',#6200,#6182);
#6186=PRODUCT_DEFINITION('Exhaust silencer envelope (1)',
'Exhaust silencer envelope (1)',#6201,#6182);
#6187=PRODUCT_DEFINITION('Hex Pipe Nipple - 1-4 Inch Tapered Pipe Thread',
'Hex Pipe Nipple - 1-4 Inch Tapered Pipe Thread',#6202,#6182);
#6188=PRODUCT_DEFINITION('Blanking plug','Blanking plug',#6203,
#6182);
#6189=PRODUCT_DEFINITION('Flush gallery plug','Flush gallery plug',
#6204,#6182);
#6190=PRODUCT_DEFINITION('Valve block','Valve block',#6205,
#6182);
#6191=PRODUCT_DEFINITION('Valve envelope','Valve envelope',#6206,
#6182);
#6192=PRODUCT_DEFINITION('Gasket plate','Gasket plate',#6207,
#6182);
#6193=PRODUCT_DEFINITION('Quarter-to-eighth-inch port reducer',
'Quarter-to-eighth-inch port reducer',#6208,#6182);
#6194=PRODUCT_DEFINITION('Push-In Tube Fitting - 6 mm Tube, 1-8 Inch Tapered Pipe Thread',
'Push-In Tube Fitting - 6 mm Tube, 1-8 Inch Tapered Pipe Thread',#6209,
#6182);
#6195=PRODUCT_DEFINITION('Body','Body',#6210,#6182);
#6196=PRODUCT_DEFINITION('Release collar','Release collar',#6211,
#6182);
#6197=PRODUCT_DEFINITION('Cap Screw - M4x16',
'Cap Screw - M4x16',#6212,#6182);
#6198=PRODUCT_DEFINITION_FORMATION('',$,#6231);
#6199=PRODUCT_DEFINITION_FORMATION('',$,#6232);
#6200=PRODUCT_DEFINITION_FORMATION('',$,#6233);
#6201=PRODUCT_DEFINITION_FORMATION('',$,#6234);
#6202=PRODUCT_DEFINITION_FORMATION('',$,#6235);
#6203=PRODUCT_DEFINITION_FORMATION('',$,#6236);
#6204=PRODUCT_DEFINITION_FORMATION('',$,#6237);
#6205=PRODUCT_DEFINITION_FORMATION('',$,#6238);
#6206=PRODUCT_DEFINITION_FORMATION('',$,#6239);
#6207=PRODUCT_DEFINITION_FORMATION('',$,#6240);
#6208=PRODUCT_DEFINITION_FORMATION('',$,#6241);
#6209=PRODUCT_DEFINITION_FORMATION('',$,#6242);
#6210=PRODUCT_DEFINITION_FORMATION('',$,#6243);
#6211=PRODUCT_DEFINITION_FORMATION('',$,#6244);
#6212=PRODUCT_DEFINITION_FORMATION('',$,#6245);
#6213=PRODUCT_RELATED_PRODUCT_CATEGORY('PAT-108',
'PAT-108',(#6231));
#6214=PRODUCT_RELATED_PRODUCT_CATEGORY('Valve sub-base',
'Valve sub-base',(#6232));
#6215=PRODUCT_RELATED_PRODUCT_CATEGORY('Exhaust silencer envelope',
'Exhaust silencer envelope',(#6233));
#6216=PRODUCT_RELATED_PRODUCT_CATEGORY('Exhaust silencer envelope (1)',
'Exhaust silencer envelope (1)',(#6234));
#6217=PRODUCT_RELATED_PRODUCT_CATEGORY(
'Hex Pipe Nipple - 1-4 Inch Tapered Pipe Thread',
'Hex Pipe Nipple - 1-4 Inch Tapered Pipe Thread',(#6235));
#6218=PRODUCT_RELATED_PRODUCT_CATEGORY('Blanking plug','Blanking plug',
(#6236));
#6219=PRODUCT_RELATED_PRODUCT_CATEGORY('Flush gallery plug',
'Flush gallery plug',(#6237));
#6220=PRODUCT_RELATED_PRODUCT_CATEGORY('Valve block','Valve block',(#6238));
#6221=PRODUCT_RELATED_PRODUCT_CATEGORY('Valve envelope',
'Valve envelope',(#6239));
#6222=PRODUCT_RELATED_PRODUCT_CATEGORY('Gasket plate','Gasket plate',(#6240));
#6223=PRODUCT_RELATED_PRODUCT_CATEGORY(
'Quarter-to-eighth-inch port reducer',
'Quarter-to-eighth-inch port reducer',(#6241));
#6224=PRODUCT_RELATED_PRODUCT_CATEGORY(
'Push-In Tube Fitting - 6 mm Tube, 1-8 Inch Tapered Pipe Thread',
'Push-In Tube Fitting - 6 mm Tube, 1-8 Inch Tapered Pipe Thread',(#6242));
#6225=PRODUCT_RELATED_PRODUCT_CATEGORY('Body','Body',(#6243));
#6226=PRODUCT_RELATED_PRODUCT_CATEGORY('Release collar',
'Release collar',(#6244));
#6227=PRODUCT_RELATED_PRODUCT_CATEGORY('Cap Screw - M4x16',
'Cap Screw - M4x16',(#6245));
#6228=APPLICATION_PROTOCOL_DEFINITION('international standard',
'automotive_design',2009,#6229);
#6229=APPLICATION_CONTEXT(
'Core Data for Automotive Mechanical Design Process');
#6230=PRODUCT_CONTEXT('part definition',#6229,'mechanical');
#6231=PRODUCT('PAT-108','PAT-108',
'PAT-108',(#6230));
#6232=PRODUCT('Valve sub-base','Valve sub-base',
'Valve sub-base',(#6230));
#6233=PRODUCT('Exhaust silencer envelope','Exhaust silencer envelope',
'Exhaust silencer envelope',(#6230));
#6234=PRODUCT('Exhaust silencer envelope (1)',
'Exhaust silencer envelope (1)','Exhaust silencer envelope (1)',(#6230));
#6235=PRODUCT('Hex Pipe Nipple - 1-4 Inch Tapered Pipe Thread',
'Hex Pipe Nipple - 1-4 Inch Tapered Pipe Thread',
'Hex Pipe Nipple - 1-4 Inch Tapered Pipe Thread',(#6230));
#6236=PRODUCT('Blanking plug','Blanking plug',
'Blanking plug',(#6230));
#6237=PRODUCT('Flush gallery plug','Flush gallery plug',
'Flush gallery plug',(#6230));
#6238=PRODUCT('Valve block','Valve block','Valve block',(#6230));
#6239=PRODUCT('Valve envelope','Valve envelope',
'Valve envelope',(#6230));
#6240=PRODUCT('Gasket plate','Gasket plate','Gasket plate',
(#6230));
#6241=PRODUCT('Quarter-to-eighth-inch port reducer',
'Quarter-to-eighth-inch port reducer',
'Quarter-to-eighth-inch port reducer',(#6230));
#6242=PRODUCT('Push-In Tube Fitting - 6 mm Tube, 1-8 Inch Tapered Pipe Thread',
'Push-In Tube Fitting - 6 mm Tube, 1-8 Inch Tapered Pipe Thread',
'Push-In Tube Fitting - 6 mm Tube, 1-8 Inch Tapered Pipe Thread',(#6230));
#6243=PRODUCT('Body','Body','Body',(#6230));
#6244=PRODUCT('Release collar','Release collar',
'Release collar',(#6230));
#6245=PRODUCT('Cap Screw - M4x16','Cap Screw - M4x16',
'Cap Screw - M4x16',(#6230));
#6246=PRESENTATION_STYLE_ASSIGNMENT((#6252));
#6247=PRESENTATION_STYLE_ASSIGNMENT((#6253));
#6248=PRESENTATION_STYLE_ASSIGNMENT((#6254));
#6249=PRESENTATION_STYLE_ASSIGNMENT((#6255));
#6250=PRESENTATION_STYLE_ASSIGNMENT((#6256));
#6251=PRESENTATION_STYLE_ASSIGNMENT((#6257));
#6252=SURFACE_STYLE_USAGE(.BOTH.,#6258);
#6253=SURFACE_STYLE_USAGE(.BOTH.,#6259);
#6254=SURFACE_STYLE_USAGE(.BOTH.,#6260);
#6255=SURFACE_STYLE_USAGE(.BOTH.,#6261);
#6256=SURFACE_STYLE_USAGE(.BOTH.,#6262);
#6257=SURFACE_STYLE_USAGE(.BOTH.,#6263);
#6258=SURFACE_SIDE_STYLE('',(#6264));
#6259=SURFACE_SIDE_STYLE('',(#6265));
#6260=SURFACE_SIDE_STYLE('',(#6266));
#6261=SURFACE_SIDE_STYLE('',(#6267));
#6262=SURFACE_SIDE_STYLE('',(#6268));
#6263=SURFACE_SIDE_STYLE('',(#6269));
#6264=SURFACE_STYLE_FILL_AREA(#6270);
#6265=SURFACE_STYLE_FILL_AREA(#6271);
#6266=SURFACE_STYLE_FILL_AREA(#6272);
#6267=SURFACE_STYLE_FILL_AREA(#6273);
#6268=SURFACE_STYLE_FILL_AREA(#6274);
#6269=SURFACE_STYLE_FILL_AREA(#6275);
#6270=FILL_AREA_STYLE('Steel - Satin',(#6276));
#6271=FILL_AREA_STYLE('CAD Library Painted - Deep blue',(#6277));
#6272=FILL_AREA_STYLE('CAD Library Painted - Engineering blue',(#6278));
#6273=FILL_AREA_STYLE('CAD Library Painted - Steel gray',(#6279));
#6274=FILL_AREA_STYLE('CAD Library Painted - Off white',(#6280));
#6275=FILL_AREA_STYLE('CAD Library Painted - Graphite',(#6281));
#6276=FILL_AREA_STYLE_COLOUR('Steel - Satin',#6282);
#6277=FILL_AREA_STYLE_COLOUR('CAD Library Painted - Deep blue',#6283);
#6278=FILL_AREA_STYLE_COLOUR('CAD Library Painted - Engineering blue',#6284);
#6279=FILL_AREA_STYLE_COLOUR('CAD Library Painted - Steel gray',#6285);
#6280=FILL_AREA_STYLE_COLOUR('CAD Library Painted - Off white',#6286);
#6281=FILL_AREA_STYLE_COLOUR('CAD Library Painted - Graphite',#6287);
#6282=COLOUR_RGB('Steel - Satin',0.627450980392157,0.627450980392157,0.627450980392157);
#6283=COLOUR_RGB('CAD Library Painted - Deep blue',0.0784313725490196,0.203921568627451,
0.349019607843137);
#6284=COLOUR_RGB('CAD Library Painted - Engineering blue',0.12156862745098,
0.356862745098039,0.6);
#6285=COLOUR_RGB('CAD Library Painted - Steel gray',0.592156862745098,0.631372549019608,
0.67843137254902);
#6286=COLOUR_RGB('CAD Library Painted - Off white',0.909803921568627,0.901960784313726,
0.858823529411765);
#6287=COLOUR_RGB('CAD Library Painted - Graphite',0.0980392156862745,0.109803921568627,
0.125490196078431);
#6288=COLOUR_RGB('Dark Blue',0.08,0.2,0.34);
#6289=FILL_AREA_STYLE_COLOUR('',#6288);
#6290=FILL_AREA_STYLE('',(#6289));
#6291=SURFACE_STYLE_FILL_AREA(#6290);
#6292=SURFACE_SIDE_STYLE('',(#6291));
#6293=SURFACE_STYLE_USAGE(.BOTH.,#6292);
#6294=PRESENTATION_STYLE_ASSIGNMENT((#6293));
#6295=COLOUR_RGB('Light Blue',0.38,0.62,0.78);
#6296=FILL_AREA_STYLE_COLOUR('',#6295);
#6297=FILL_AREA_STYLE('',(#6296));
#6298=SURFACE_STYLE_FILL_AREA(#6297);
#6299=SURFACE_SIDE_STYLE('',(#6298));
#6300=SURFACE_STYLE_USAGE(.BOTH.,#6299);
#6301=PRESENTATION_STYLE_ASSIGNMENT((#6300));
#6302=COLOUR_RGB('Sky Blue',0.24,0.69,0.87);
#6303=FILL_AREA_STYLE_COLOUR('',#6302);
#6304=FILL_AREA_STYLE('',(#6303));
#6305=SURFACE_STYLE_FILL_AREA(#6304);
#6306=SURFACE_SIDE_STYLE('',(#6305));
#6307=SURFACE_STYLE_USAGE(.BOTH.,#6306);
#6308=PRESENTATION_STYLE_ASSIGNMENT((#6307));
#6309=COLOUR_RGB('Grey',0.48,0.52,0.57);
#6310=FILL_AREA_STYLE_COLOUR('',#6309);
#6311=FILL_AREA_STYLE('',(#6310));
#6312=SURFACE_STYLE_FILL_AREA(#6311);
#6313=SURFACE_SIDE_STYLE('',(#6312));
#6314=SURFACE_STYLE_USAGE(.BOTH.,#6313);
#6315=PRESENTATION_STYLE_ASSIGNMENT((#6314));
#6316=COLOUR_RGB('Black',0.12,0.14,0.17);
#6317=FILL_AREA_STYLE_COLOUR('',#6316);
#6318=FILL_AREA_STYLE('',(#6317));
#6319=SURFACE_STYLE_FILL_AREA(#6318);
#6320=SURFACE_SIDE_STYLE('',(#6319));
#6321=SURFACE_STYLE_USAGE(.BOTH.,#6320);
#6322=PRESENTATION_STYLE_ASSIGNMENT((#6321));
#6323=COLOUR_RGB('Off White',0.89,0.88,0.83);
#6324=FILL_AREA_STYLE_COLOUR('',#6323);
#6325=FILL_AREA_STYLE('',(#6324));
#6326=SURFACE_STYLE_FILL_AREA(#6325);
#6327=SURFACE_SIDE_STYLE('',(#6326));
#6328=SURFACE_STYLE_USAGE(.BOTH.,#6327);
#6329=PRESENTATION_STYLE_ASSIGNMENT((#6328));
ENDSEC;
END-ISO-10303-21;
